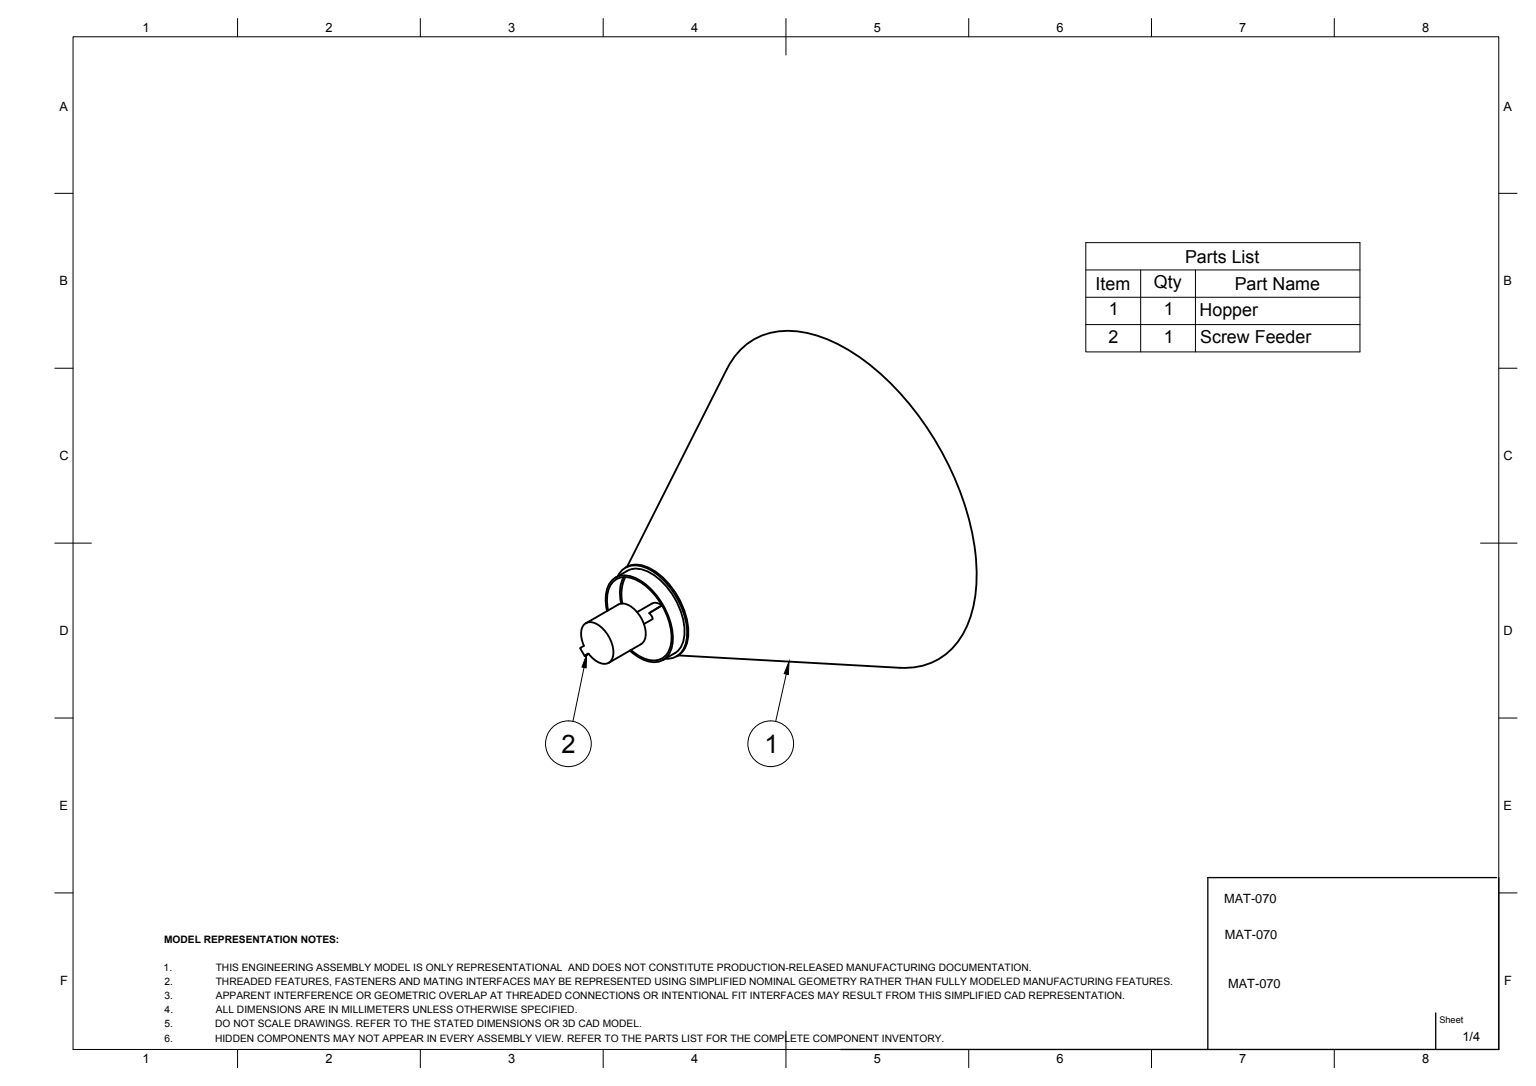
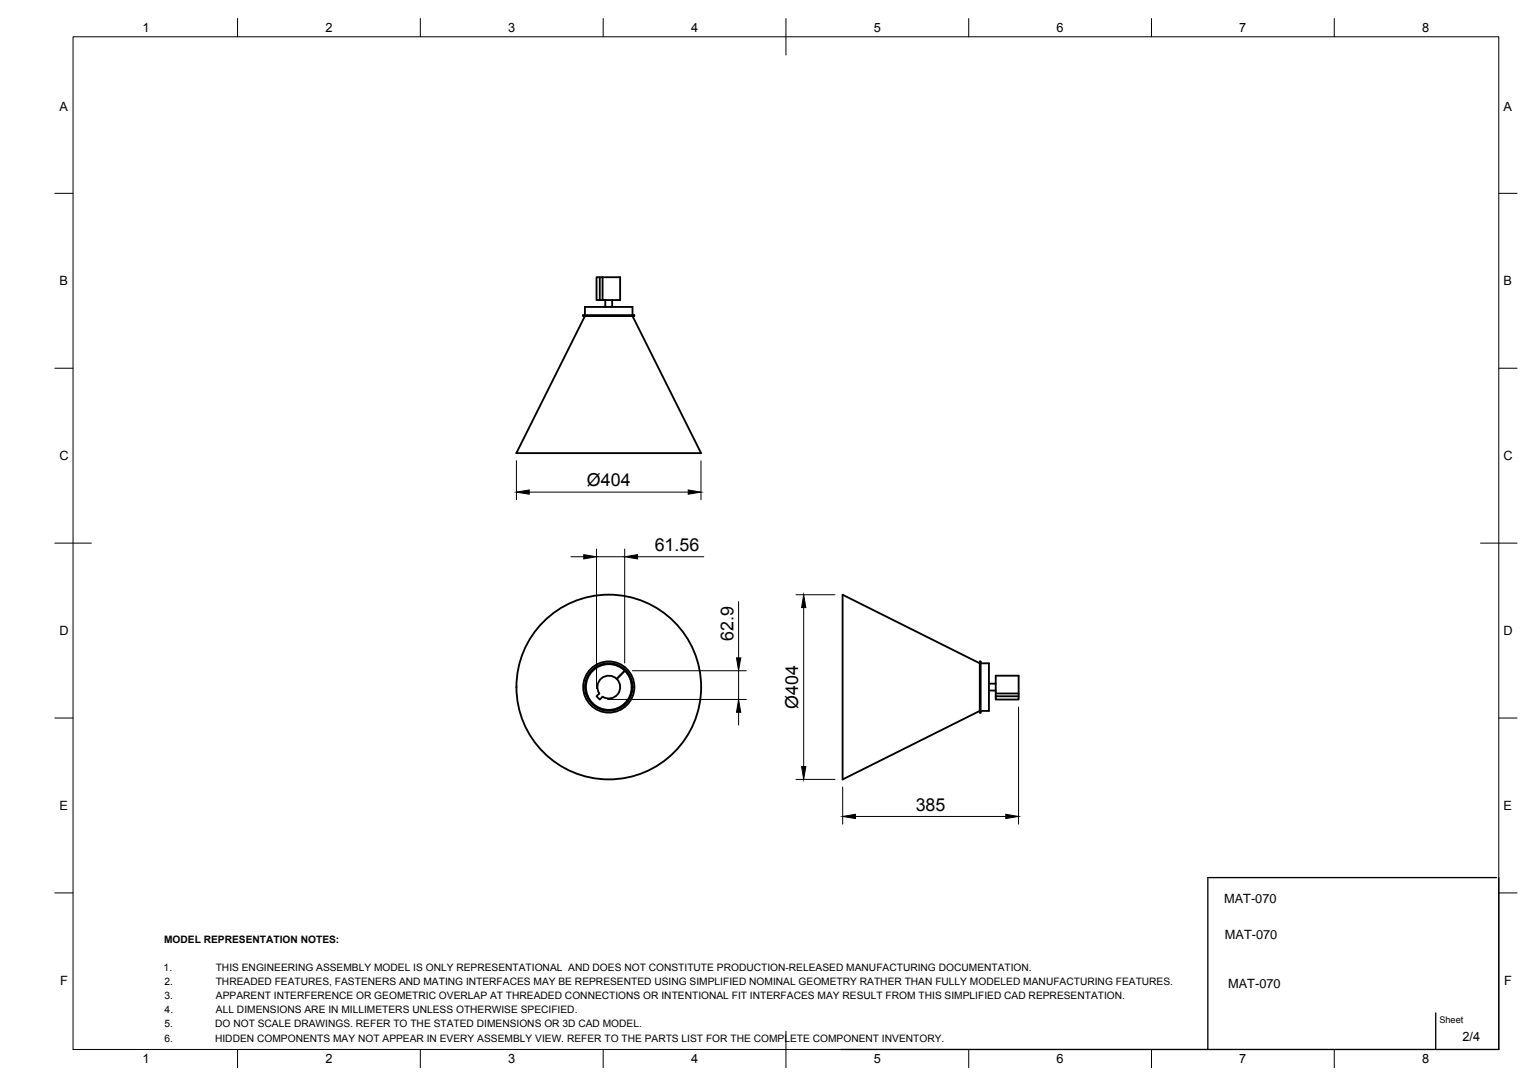
ISO-10303-21;
HEADER;
/* Generated by software containing ST-Developer
 * from STEP Tools, Inc. (www.steptools.com) 
 */

FILE_DESCRIPTION(
/* description */ (''),
/* implementation_level */ '2;1');

FILE_NAME(
/* name */ 'MAT-070',
/* time_stamp */ '2026-10-24T12:18:10-07:00',
/* author */ (''),
/* organization */ (''),
/* preprocessor_version */ 'ST-DEVELOPER v20.2',
/* originating_system */ 'Autodesk Translation Framework v15.15.0.0',
/* authorisation */ '');

FILE_SCHEMA (('AUTOMOTIVE_DESIGN { 1 0 10303 214 3 1 1 }'));
ENDSEC;

DATA;
#10=MECHANICAL_DESIGN_GEOMETRIC_PRESENTATION_REPRESENTATION('',(#38,#39),
#2858);
#11=ITEM_DEFINED_TRANSFORMATION($,$,#415,#453);
#12=ITEM_DEFINED_TRANSFORMATION($,$,#434,#454);
#13=(
REPRESENTATION_RELATIONSHIP($,$,#2872,#2871)
REPRESENTATION_RELATIONSHIP_WITH_TRANSFORMATION(#11)
SHAPE_REPRESENTATION_RELATIONSHIP()
);
#14=(
REPRESENTATION_RELATIONSHIP($,$,#2873,#2871)
REPRESENTATION_RELATIONSHIP_WITH_TRANSFORMATION(#12)
SHAPE_REPRESENTATION_RELATIONSHIP()
);
#15=CONTEXT_DEPENDENT_SHAPE_REPRESENTATION(#13,#2869);
#16=CONTEXT_DEPENDENT_SHAPE_REPRESENTATION(#14,#2870);
#17=NEXT_ASSEMBLY_USAGE_OCCURRENCE('Hopper:1','Hopper:1','Hopper:1',#2875,
#2876,'Hopper:1');
#18=NEXT_ASSEMBLY_USAGE_OCCURRENCE('Screw Feeder:1','Screw Feeder:1',
'Screw Feeder:1',#2875,#2877,'Screw Feeder:1');
#19=(
BOUNDED_SURFACE()
B_SPLINE_SURFACE(1,2,((#1855,#1856,#1857,#1858,#1859,#1860,#1861,#1862,
#1863,#1864,#1865,#1866,#1867,#1868,#1869,#1870,#1871,#1872,#1873,#1874,
#1875,#1876,#1877,#1878,#1879,#1880,#1881,#1882,#1883,#1884,#1885,#1886,
#1887,#1888,#1889,#1890,#1891,#1892,#1893,#1894,#1895,#1896,#1897,#1898,
#1899,#1900,#1901,#1902,#1903,#1904,#1905,#1906,#1907,#1908,#1909,#1910,
#1911,#1912,#1913,#1914,#1915,#1916,#1917,#1918,#1919,#1920,#1921,#1922,
#1923,#1924,#1925,#1926,#1927,#1928,#1929,#1930,#1931,#1932,#1933,#1934,
#1935,#1936,#1937,#1938,#1939,#1940,#1941,#1942,#1943,#1944,#1945,#1946,
#1947,#1948,#1949,#1950,#1951,#1952,#1953,#1954,#1955,#1956,#1957,#1958,
#1959,#1960,#1961,#1962,#1963,#1964,#1965,#1966,#1967,#1968,#1969,#1970,
#1971,#1972,#1973,#1974,#1975),(#1976,#1977,#1978,#1979,#1980,#1981,#1982,
#1983,#1984,#1985,#1986,#1987,#1988,#1989,#1990,#1991,#1992,#1993,#1994,
#1995,#1996,#1997,#1998,#1999,#2000,#2001,#2002,#2003,#2004,#2005,#2006,
#2007,#2008,#2009,#2010,#2011,#2012,#2013,#2014,#2015,#2016,#2017,#2018,
#2019,#2020,#2021,#2022,#2023,#2024,#2025,#2026,#2027,#2028,#2029,#2030,
#2031,#2032,#2033,#2034,#2035,#2036,#2037,#2038,#2039,#2040,#2041,#2042,
#2043,#2044,#2045,#2046,#2047,#2048,#2049,#2050,#2051,#2052,#2053,#2054,
#2055,#2056,#2057,#2058,#2059,#2060,#2061,#2062,#2063,#2064,#2065,#2066,
#2067,#2068,#2069,#2070,#2071,#2072,#2073,#2074,#2075,#2076,#2077,#2078,
#2079,#2080,#2081,#2082,#2083,#2084,#2085,#2086,#2087,#2088,#2089,#2090,
#2091,#2092,#2093,#2094,#2095,#2096)),.UNSPECIFIED.,.F.,.F.,.F.)
B_SPLINE_SURFACE_WITH_KNOTS((2,2),(3,2,2,2,2,2,2,2,2,2,2,2,2,2,2,2,2,2,
2,2,2,2,2,2,2,2,2,2,2,2,2,2,2,2,2,2,2,2,2,2,2,2,2,2,2,2,2,2,2,2,2,2,2,2,
2,2,2,2,2,2,3),(0.,1.),(0.,0.0166666666666667,0.0333333333333333,0.05,0.0666666666666667,
0.0833333333333333,0.1,0.116666666666667,0.133333333333333,0.15,0.166666666666667,
0.183333333333333,0.2,0.216666666666667,0.233333333333333,0.25,0.266666666666667,
0.283333333333333,0.3,0.316666666666667,0.333333333333333,0.35,0.366666666666667,
0.383333333333333,0.4,0.416666666666667,0.433333333333333,0.45,0.466666666666667,
0.483333333333333,0.5,0.516666666666667,0.533333333333333,0.55,0.566666666666667,
0.583333333333333,0.6,0.616666666666667,0.633333333333333,0.65,0.666666666666667,
0.683333333333333,0.7,0.716666666666667,0.733333333333333,0.75,0.766666666666667,
0.783333333333333,0.8,0.816666666666667,0.833333333333333,0.85,0.866666666666667,
0.883333333333333,0.9,0.916666666666667,0.933333333333333,0.95,0.966666666666667,
0.983333333333333,1.),.UNSPECIFIED.)
GEOMETRIC_REPRESENTATION_ITEM()
RATIONAL_B_SPLINE_SURFACE(((1.,0.987688340595138,1.,0.987688340595138,1.,
0.987688340595138,1.,0.987688340595138,1.,0.987688340595138,1.,0.987688340595138,
1.,0.987688340595138,1.,0.987688340595138,1.,0.987688340595138,1.,0.987688340595138,
1.,0.987688340595138,1.,0.987688340595138,1.,0.987688340595138,1.,0.987688340595138,
1.,0.987688340595138,1.,0.987688340595138,1.,0.987688340595138,1.,0.987688340595138,
1.,0.987688340595138,1.,0.987688340595138,1.,0.987688340595138,1.,0.987688340595138,
1.,0.987688340595138,1.,0.987688340595138,1.,0.987688340595138,1.,0.987688340595138,
1.,0.987688340595138,1.,0.987688340595138,1.,0.987688340595138,1.,0.987688340595138,
1.,0.987688340595138,1.,0.987688340595138,1.,0.987688340595138,1.,0.987688340595138,
1.,0.987688340595138,1.,0.987688340595138,1.,0.987688340595138,1.,0.987688340595138,
1.,0.987688340595138,1.,0.987688340595138,1.,0.987688340595138,1.,0.987688340595138,
1.,0.987688340595138,1.,0.987688340595138,1.,0.987688340595138,1.,0.987688340595138,
1.,0.987688340595138,1.,0.987688340595138,1.,0.987688340595138,1.,0.987688340595138,
1.,0.987688340595138,1.,0.987688340595138,1.,0.987688340595138,1.,0.987688340595138,
1.,0.987688340595138,1.,0.987688340595138,1.,0.987688340595138,1.,0.987688340595138,
1.,0.987688340595138,1.,0.987688340595138,1.),(1.,0.987688340595138,1.,
0.987688340595138,1.,0.987688340595138,1.,0.987688340595138,1.,0.987688340595138,
1.,0.987688340595138,1.,0.987688340595138,1.,0.987688340595138,1.,0.987688340595138,
1.,0.987688340595138,1.,0.987688340595138,1.,0.987688340595138,1.,0.987688340595138,
1.,0.987688340595138,1.,0.987688340595138,1.,0.987688340595138,1.,0.987688340595138,
1.,0.987688340595138,1.,0.987688340595138,1.,0.987688340595138,1.,0.987688340595138,
1.,0.987688340595138,1.,0.987688340595138,1.,0.987688340595138,1.,0.987688340595138,
1.,0.987688340595138,1.,0.987688340595138,1.,0.987688340595138,1.,0.987688340595138,
1.,0.987688340595138,1.,0.987688340595138,1.,0.987688340595138,1.,0.987688340595138,
1.,0.987688340595138,1.,0.987688340595138,1.,0.987688340595138,1.,0.987688340595138,
1.,0.987688340595138,1.,0.987688340595138,1.,0.987688340595138,1.,0.987688340595138,
1.,0.987688340595138,1.,0.987688340595138,1.,0.987688340595138,1.,0.987688340595138,
1.,0.987688340595138,1.,0.987688340595138,1.,0.987688340595138,1.,0.987688340595138,
1.,0.987688340595138,1.,0.987688340595138,1.,0.987688340595138,1.,0.987688340595138,
1.,0.987688340595138,1.,0.987688340595138,1.,0.987688340595138,1.,0.987688340595138,
1.,0.987688340595138,1.,0.987688340595138,1.,0.987688340595138,1.)))
REPRESENTATION_ITEM('')
SURFACE()
);
#20=(
BOUNDED_SURFACE()
B_SPLINE_SURFACE(1,2,((#2218,#2219,#2220,#2221,#2222,#2223,#2224,#2225,
#2226,#2227,#2228,#2229,#2230,#2231,#2232,#2233,#2234,#2235,#2236,#2237,
#2238,#2239,#2240,#2241,#2242,#2243,#2244,#2245,#2246,#2247,#2248,#2249,
#2250,#2251,#2252,#2253,#2254,#2255,#2256,#2257,#2258,#2259,#2260,#2261,
#2262,#2263,#2264,#2265,#2266,#2267,#2268,#2269,#2270,#2271,#2272,#2273,
#2274,#2275,#2276,#2277,#2278,#2279,#2280,#2281,#2282,#2283,#2284,#2285,
#2286,#2287,#2288,#2289,#2290,#2291,#2292,#2293,#2294,#2295,#2296,#2297,
#2298,#2299,#2300,#2301,#2302,#2303,#2304,#2305,#2306,#2307,#2308,#2309,
#2310,#2311,#2312,#2313,#2314,#2315,#2316,#2317,#2318,#2319,#2320,#2321,
#2322,#2323,#2324,#2325,#2326,#2327,#2328,#2329,#2330,#2331,#2332,#2333,
#2334,#2335,#2336,#2337,#2338),(#2339,#2340,#2341,#2342,#2343,#2344,#2345,
#2346,#2347,#2348,#2349,#2350,#2351,#2352,#2353,#2354,#2355,#2356,#2357,
#2358,#2359,#2360,#2361,#2362,#2363,#2364,#2365,#2366,#2367,#2368,#2369,
#2370,#2371,#2372,#2373,#2374,#2375,#2376,#2377,#2378,#2379,#2380,#2381,
#2382,#2383,#2384,#2385,#2386,#2387,#2388,#2389,#2390,#2391,#2392,#2393,
#2394,#2395,#2396,#2397,#2398,#2399,#2400,#2401,#2402,#2403,#2404,#2405,
#2406,#2407,#2408,#2409,#2410,#2411,#2412,#2413,#2414,#2415,#2416,#2417,
#2418,#2419,#2420,#2421,#2422,#2423,#2424,#2425,#2426,#2427,#2428,#2429,
#2430,#2431,#2432,#2433,#2434,#2435,#2436,#2437,#2438,#2439,#2440,#2441,
#2442,#2443,#2444,#2445,#2446,#2447,#2448,#2449,#2450,#2451,#2452,#2453,
#2454,#2455,#2456,#2457,#2458,#2459)),.UNSPECIFIED.,.F.,.F.,.F.)
B_SPLINE_SURFACE_WITH_KNOTS((2,2),(3,2,2,2,2,2,2,2,2,2,2,2,2,2,2,2,2,2,
2,2,2,2,2,2,2,2,2,2,2,2,2,2,2,2,2,2,2,2,2,2,2,2,2,2,2,2,2,2,2,2,2,2,2,2,
2,2,2,2,2,2,3),(0.,1.),(0.,0.0166666666666667,0.0333333333333333,0.05,0.0666666666666667,
0.0833333333333333,0.1,0.116666666666667,0.133333333333333,0.15,0.166666666666667,
0.183333333333333,0.2,0.216666666666667,0.233333333333333,0.25,0.266666666666667,
0.283333333333333,0.3,0.316666666666667,0.333333333333333,0.35,0.366666666666667,
0.383333333333333,0.4,0.416666666666667,0.433333333333333,0.45,0.466666666666667,
0.483333333333333,0.5,0.516666666666667,0.533333333333333,0.55,0.566666666666667,
0.583333333333333,0.6,0.616666666666667,0.633333333333333,0.65,0.666666666666667,
0.683333333333333,0.7,0.716666666666667,0.733333333333333,0.75,0.766666666666667,
0.783333333333333,0.8,0.816666666666667,0.833333333333333,0.85,0.866666666666667,
0.883333333333333,0.9,0.916666666666667,0.933333333333333,0.95,0.966666666666667,
0.983333333333333,1.),.UNSPECIFIED.)
GEOMETRIC_REPRESENTATION_ITEM()
RATIONAL_B_SPLINE_SURFACE(((1.,0.987688340595138,1.,0.987688340595138,1.,
0.987688340595138,1.,0.987688340595138,1.,0.987688340595138,1.,0.987688340595138,
1.,0.987688340595138,1.,0.987688340595138,1.,0.987688340595138,1.,0.987688340595138,
1.,0.987688340595138,1.,0.987688340595138,1.,0.987688340595138,1.,0.987688340595138,
1.,0.987688340595138,1.,0.987688340595138,1.,0.987688340595138,1.,0.987688340595138,
1.,0.987688340595138,1.,0.987688340595138,1.,0.987688340595138,1.,0.987688340595138,
1.,0.987688340595138,1.,0.987688340595138,1.,0.987688340595138,1.,0.987688340595138,
1.,0.987688340595138,1.,0.987688340595138,1.,0.987688340595138,1.,0.987688340595138,
1.,0.987688340595138,1.,0.987688340595138,1.,0.987688340595138,1.,0.987688340595138,
1.,0.987688340595138,1.,0.987688340595138,1.,0.987688340595138,1.,0.987688340595138,
1.,0.987688340595138,1.,0.987688340595138,1.,0.987688340595138,1.,0.987688340595138,
1.,0.987688340595138,1.,0.987688340595138,1.,0.987688340595138,1.,0.987688340595138,
1.,0.987688340595138,1.,0.987688340595138,1.,0.987688340595138,1.,0.987688340595138,
1.,0.987688340595138,1.,0.987688340595138,1.,0.987688340595138,1.,0.987688340595138,
1.,0.987688340595138,1.,0.987688340595138,1.,0.987688340595138,1.,0.987688340595138,
1.,0.987688340595138,1.,0.987688340595138,1.),(1.,0.987688340595138,1.,
0.987688340595138,1.,0.987688340595138,1.,0.987688340595138,1.,0.987688340595138,
1.,0.987688340595138,1.,0.987688340595138,1.,0.987688340595138,1.,0.987688340595138,
1.,0.987688340595138,1.,0.987688340595138,1.,0.987688340595138,1.,0.987688340595138,
1.,0.987688340595138,1.,0.987688340595138,1.,0.987688340595138,1.,0.987688340595138,
1.,0.987688340595138,1.,0.987688340595138,1.,0.987688340595138,1.,0.987688340595138,
1.,0.987688340595138,1.,0.987688340595138,1.,0.987688340595138,1.,0.987688340595138,
1.,0.987688340595138,1.,0.987688340595138,1.,0.987688340595138,1.,0.987688340595138,
1.,0.987688340595138,1.,0.987688340595138,1.,0.987688340595138,1.,0.987688340595138,
1.,0.987688340595138,1.,0.987688340595138,1.,0.987688340595138,1.,0.987688340595138,
1.,0.987688340595138,1.,0.987688340595138,1.,0.987688340595138,1.,0.987688340595138,
1.,0.987688340595138,1.,0.987688340595138,1.,0.987688340595138,1.,0.987688340595138,
1.,0.987688340595138,1.,0.987688340595138,1.,0.987688340595138,1.,0.987688340595138,
1.,0.987688340595138,1.,0.987688340595138,1.,0.987688340595138,1.,0.987688340595138,
1.,0.987688340595138,1.,0.987688340595138,1.,0.987688340595138,1.,0.987688340595138,
1.,0.987688340595138,1.,0.987688340595138,1.,0.987688340595138,1.)))
REPRESENTATION_ITEM('')
SURFACE()
);
#21=(
BOUNDED_SURFACE()
B_SPLINE_SURFACE(1,2,((#2581,#2582,#2583,#2584,#2585,#2586,#2587,#2588,
#2589,#2590,#2591,#2592,#2593,#2594,#2595,#2596,#2597,#2598,#2599,#2600,
#2601,#2602,#2603,#2604,#2605,#2606,#2607,#2608,#2609,#2610,#2611,#2612,
#2613,#2614,#2615,#2616,#2617,#2618,#2619,#2620,#2621,#2622,#2623,#2624,
#2625,#2626,#2627,#2628,#2629,#2630,#2631,#2632,#2633,#2634,#2635,#2636,
#2637,#2638,#2639,#2640,#2641,#2642,#2643,#2644,#2645,#2646,#2647,#2648,
#2649,#2650,#2651,#2652,#2653,#2654,#2655,#2656,#2657,#2658,#2659,#2660,
#2661,#2662,#2663,#2664,#2665,#2666,#2667,#2668,#2669,#2670,#2671,#2672,
#2673,#2674,#2675,#2676,#2677,#2678,#2679,#2680,#2681,#2682,#2683,#2684,
#2685,#2686,#2687,#2688,#2689,#2690,#2691,#2692,#2693,#2694,#2695,#2696,
#2697,#2698,#2699,#2700,#2701),(#2702,#2703,#2704,#2705,#2706,#2707,#2708,
#2709,#2710,#2711,#2712,#2713,#2714,#2715,#2716,#2717,#2718,#2719,#2720,
#2721,#2722,#2723,#2724,#2725,#2726,#2727,#2728,#2729,#2730,#2731,#2732,
#2733,#2734,#2735,#2736,#2737,#2738,#2739,#2740,#2741,#2742,#2743,#2744,
#2745,#2746,#2747,#2748,#2749,#2750,#2751,#2752,#2753,#2754,#2755,#2756,
#2757,#2758,#2759,#2760,#2761,#2762,#2763,#2764,#2765,#2766,#2767,#2768,
#2769,#2770,#2771,#2772,#2773,#2774,#2775,#2776,#2777,#2778,#2779,#2780,
#2781,#2782,#2783,#2784,#2785,#2786,#2787,#2788,#2789,#2790,#2791,#2792,
#2793,#2794,#2795,#2796,#2797,#2798,#2799,#2800,#2801,#2802,#2803,#2804,
#2805,#2806,#2807,#2808,#2809,#2810,#2811,#2812,#2813,#2814,#2815,#2816,
#2817,#2818,#2819,#2820,#2821,#2822)),.UNSPECIFIED.,.F.,.F.,.F.)
B_SPLINE_SURFACE_WITH_KNOTS((2,2),(3,2,2,2,2,2,2,2,2,2,2,2,2,2,2,2,2,2,
2,2,2,2,2,2,2,2,2,2,2,2,2,2,2,2,2,2,2,2,2,2,2,2,2,2,2,2,2,2,2,2,2,2,2,2,
2,2,2,2,2,2,3),(0.,1.),(0.,0.0166666666666667,0.0333333333333333,0.05,0.0666666666666667,
0.0833333333333333,0.1,0.116666666666667,0.133333333333333,0.15,0.166666666666667,
0.183333333333333,0.2,0.216666666666667,0.233333333333333,0.25,0.266666666666667,
0.283333333333333,0.3,0.316666666666667,0.333333333333333,0.35,0.366666666666667,
0.383333333333333,0.4,0.416666666666667,0.433333333333333,0.45,0.466666666666667,
0.483333333333333,0.5,0.516666666666667,0.533333333333333,0.55,0.566666666666667,
0.583333333333333,0.6,0.616666666666667,0.633333333333333,0.65,0.666666666666667,
0.683333333333333,0.7,0.716666666666667,0.733333333333333,0.75,0.766666666666667,
0.783333333333333,0.8,0.816666666666667,0.833333333333333,0.85,0.866666666666667,
0.883333333333333,0.9,0.916666666666667,0.933333333333333,0.95,0.966666666666667,
0.983333333333333,1.),.UNSPECIFIED.)
GEOMETRIC_REPRESENTATION_ITEM()
RATIONAL_B_SPLINE_SURFACE(((1.,0.987688340595138,1.,0.987688340595138,1.,
0.987688340595138,1.,0.987688340595138,1.,0.987688340595138,1.,0.987688340595138,
1.,0.987688340595138,1.,0.987688340595138,1.,0.987688340595138,1.,0.987688340595138,
1.,0.987688340595138,1.,0.987688340595138,1.,0.987688340595138,1.,0.987688340595138,
1.,0.987688340595138,1.,0.987688340595138,1.,0.987688340595138,1.,0.987688340595138,
1.,0.987688340595138,1.,0.987688340595138,1.,0.987688340595138,1.,0.987688340595138,
1.,0.987688340595138,1.,0.987688340595138,1.,0.987688340595138,1.,0.987688340595138,
1.,0.987688340595138,1.,0.987688340595138,1.,0.987688340595138,1.,0.987688340595138,
1.,0.987688340595138,1.,0.987688340595138,1.,0.987688340595138,1.,0.987688340595138,
1.,0.987688340595138,1.,0.987688340595138,1.,0.987688340595138,1.,0.987688340595138,
1.,0.987688340595138,1.,0.987688340595138,1.,0.987688340595138,1.,0.987688340595138,
1.,0.987688340595138,1.,0.987688340595138,1.,0.987688340595138,1.,0.987688340595138,
1.,0.987688340595138,1.,0.987688340595138,1.,0.987688340595138,1.,0.987688340595138,
1.,0.987688340595138,1.,0.987688340595138,1.,0.987688340595138,1.,0.987688340595138,
1.,0.987688340595138,1.,0.987688340595138,1.,0.987688340595138,1.,0.987688340595138,
1.,0.987688340595138,1.,0.987688340595138,1.),(1.,0.987688340595138,1.,
0.987688340595138,1.,0.987688340595138,1.,0.987688340595138,1.,0.987688340595138,
1.,0.987688340595138,1.,0.987688340595138,1.,0.987688340595138,1.,0.987688340595138,
1.,0.987688340595138,1.,0.987688340595138,1.,0.987688340595138,1.,0.987688340595138,
1.,0.987688340595138,1.,0.987688340595138,1.,0.987688340595138,1.,0.987688340595138,
1.,0.987688340595138,1.,0.987688340595138,1.,0.987688340595138,1.,0.987688340595138,
1.,0.987688340595138,1.,0.987688340595138,1.,0.987688340595138,1.,0.987688340595138,
1.,0.987688340595138,1.,0.987688340595138,1.,0.987688340595138,1.,0.987688340595138,
1.,0.987688340595138,1.,0.987688340595138,1.,0.987688340595138,1.,0.987688340595138,
1.,0.987688340595138,1.,0.987688340595138,1.,0.987688340595138,1.,0.987688340595138,
1.,0.987688340595138,1.,0.987688340595138,1.,0.987688340595138,1.,0.987688340595138,
1.,0.987688340595138,1.,0.987688340595138,1.,0.987688340595138,1.,0.987688340595138,
1.,0.987688340595138,1.,0.987688340595138,1.,0.987688340595138,1.,0.987688340595138,
1.,0.987688340595138,1.,0.987688340595138,1.,0.987688340595138,1.,0.987688340595138,
1.,0.987688340595138,1.,0.987688340595138,1.,0.987688340595138,1.,0.987688340595138,
1.,0.987688340595138,1.,0.987688340595138,1.,0.987688340595138,1.)))
REPRESENTATION_ITEM('')
SURFACE()
);
#22=B_SPLINE_CURVE_WITH_KNOTS('',3,(#652,#653,#654,#655),.UNSPECIFIED.,
 .F.,.F.,(4,4),(-1.,-0.998645968698766),.UNSPECIFIED.);
#23=B_SPLINE_CURVE_WITH_KNOTS('',3,(#662,#663,#664,#665,#666,#667,#668,
#669,#670,#671,#672,#673,#674,#675,#676,#677,#678,#679,#680,#681,#682,#683,
#684,#685,#686,#687,#688,#689,#690,#691,#692,#693,#694,#695,#696,#697,#698,
#699,#700,#701,#702,#703,#704,#705,#706,#707,#708,#709,#710,#711,#712,#713,
#714,#715,#716,#717,#718,#719,#720,#721,#722,#723,#724,#725,#726,#727,#728,
#729,#730,#731,#732,#733,#734,#735,#736,#737,#738,#739,#740,#741,#742,#743,
#744,#745,#746,#747,#748,#749,#750,#751,#752,#753,#754,#755,#756,#757,#758,
#759,#760,#761,#762,#763,#764,#765,#766,#767,#768,#769,#770,#771,#772,#773,
#774,#775,#776,#777,#778,#779,#780,#781,#782,#783,#784,#785,#786,#787,#788,
#789,#790,#791,#792,#793,#794,#795,#796,#797,#798,#799,#800,#801,#802,#803,
#804,#805,#806,#807,#808,#809,#810,#811,#812,#813,#814,#815,#816,#817,#818,
#819,#820,#821,#822,#823,#824,#825,#826,#827,#828,#829,#830,#831,#832,#833,
#834,#835,#836,#837,#838,#839,#840,#841,#842,#843,#844,#845,#846,#847,#848,
#849,#850,#851,#852,#853,#854,#855,#856,#857,#858,#859,#860,#861,#862,#863,
#864,#865,#866,#867,#868,#869,#870,#871,#872,#873,#874,#875,#876,#877,#878,
#879,#880,#881,#882,#883,#884,#885,#886,#887,#888,#889,#890,#891,#892,#893,
#894,#895,#896,#897,#898,#899,#900,#901,#902,#903,#904,#905,#906,#907,#908,
#909,#910,#911,#912,#913,#914,#915,#916,#917,#918,#919,#920,#921,#922,#923,
#924,#925,#926,#927,#928,#929,#930,#931,#932,#933,#934,#935,#936,#937,#938,
#939,#940,#941,#942,#943,#944,#945,#946,#947,#948,#949,#950,#951,#952,#953,
#954,#955,#956,#957,#958,#959,#960,#961,#962,#963,#964,#965,#966,#967,#968,
#969,#970,#971,#972,#973,#974,#975,#976,#977,#978,#979,#980,#981,#982,#983,
#984,#985,#986,#987,#988,#989,#990,#991,#992,#993,#994,#995,#996,#997,#998,
#999,#1000,#1001,#1002,#1003,#1004,#1005,#1006,#1007,#1008,#1009,#1010,
#1011,#1012,#1013,#1014,#1015,#1016,#1017,#1018,#1019),.UNSPECIFIED.,.F.,
 .F.,(4,3,3,3,3,3,3,3,3,3,3,3,3,3,3,3,3,3,3,3,3,3,3,3,3,3,3,3,3,3,3,3,3,
3,3,3,3,3,3,3,3,3,3,3,3,3,3,3,3,3,3,3,3,3,3,3,3,3,3,3,3,3,3,3,3,3,3,3,3,
3,3,3,3,3,3,3,3,3,3,3,3,3,3,3,3,3,3,3,3,3,3,3,3,3,3,3,3,3,3,3,3,3,3,3,3,
3,3,3,3,3,3,3,3,3,3,3,3,3,3,4),(-0.331979302032099,-0.328745544947817,-0.325511126349503,
-0.322277581756429,-0.319042795051795,-0.316666666666667,-0.313432410645245,
-0.310074307983934,-0.306840488099785,-0.303607230746873,-0.300373105768056,
-0.3,-0.296765743978578,-0.293407641317267,-0.290173821433118,-0.286940564080179,
-0.283706439101408,-0.283333333333333,-0.280099077311897,-0.27674097465059,
-0.273507154766441,-0.270273897413541,-0.267039772434759,-0.266666666666667,
-0.263432410645244,-0.260074307983933,-0.25684048809978,-0.253607230746841,
-0.250373105768036,-0.25,-0.246765743978575,-0.243407641317264,-0.240173821433105,
-0.236940564080198,-0.233706439101398,-0.233333333333333,-0.230099077311924,
-0.22674097465061,-0.223507154766454,-0.220273897413536,-0.217039772434708,
-0.216666666666667,-0.213432410645268,-0.210074307983951,-0.206840488099798,
-0.203607230746877,-0.200373105768084,-0.2,-0.196765743978578,-0.193407641317267,
-0.190173821433123,-0.186940564080229,-0.183706439101414,-0.183333333333333,
-0.180099077311908,-0.176740974650597,-0.173507154766428,-0.170273897413483,
-0.167039772434678,-0.166666666666667,-0.163432410645259,-0.160074307983944,
-0.156840488099797,-0.153607230746853,-0.150373105768069,-0.15,-0.146765743978574,
-0.143407641317264,-0.140173821433101,-0.136940564080169,-0.133706439101386,
-0.133333333333333,-0.130099077311911,-0.1267409746506,-0.123507154766447,
-0.120273897413526,-0.117039772434722,-0.116666666666667,-0.113432410645241,
-0.110074307983931,-0.106840488099774,-0.103607230746858,-0.10037310576804,
-0.1,-0.0967657439785776,-0.0934076413172665,-0.0901738214331063,-0.0869405640801917,
-0.0837064391013879,-0.0833333333333334,-0.0800990773119075,-0.0767409746505973,
-0.0735071547664396,-0.0702738974135466,-0.0670397724347522,-0.0666666666666667,
-0.0634324106452447,-0.0600743079839336,-0.0568404880997839,-0.0536072307468639,
-0.0503731057680767,-0.05,-0.0467657439785748,-0.0434076413172644,-0.0401738214331216,
-0.0369405640801967,-0.033706439101418,-0.0333333333333333,-0.030099077311911,
-0.0267409746505999,-0.0235071547664523,-0.0202738974135343,-0.017039772434738,
-0.0166666666666667,-0.0134324106517174,-0.0100743318149406,-0.00684051195133032,
-0.00360725461687006,-0.000373129688631168,-9.53046099950368E-8),
 .UNSPECIFIED.);
#24=B_SPLINE_CURVE_WITH_KNOTS('',3,(#1066,#1067,#1068,#1069,#1070,#1071,
#1072,#1073,#1074,#1075,#1076,#1077,#1078,#1079,#1080,#1081,#1082,#1083,
#1084,#1085,#1086,#1087,#1088,#1089,#1090,#1091,#1092,#1093,#1094,#1095,
#1096,#1097,#1098,#1099,#1100,#1101,#1102,#1103,#1104,#1105,#1106,#1107,
#1108,#1109,#1110,#1111,#1112,#1113,#1114,#1115,#1116,#1117,#1118,#1119,
#1120,#1121,#1122,#1123,#1124,#1125,#1126,#1127,#1128,#1129,#1130,#1131,
#1132,#1133,#1134,#1135,#1136,#1137,#1138,#1139,#1140,#1141,#1142,#1143,
#1144,#1145,#1146,#1147,#1148,#1149,#1150,#1151,#1152,#1153,#1154,#1155,
#1156,#1157,#1158,#1159,#1160,#1161,#1162,#1163,#1164,#1165,#1166,#1167,
#1168,#1169,#1170,#1171,#1172,#1173,#1174,#1175,#1176,#1177,#1178,#1179,
#1180,#1181,#1182,#1183,#1184,#1185,#1186,#1187,#1188,#1189,#1190,#1191,
#1192,#1193,#1194,#1195,#1196,#1197,#1198,#1199,#1200,#1201,#1202,#1203,
#1204,#1205,#1206,#1207,#1208,#1209,#1210,#1211,#1212,#1213,#1214,#1215,
#1216,#1217,#1218,#1219,#1220,#1221,#1222,#1223,#1224,#1225,#1226,#1227,
#1228,#1229,#1230,#1231,#1232,#1233,#1234,#1235,#1236,#1237,#1238,#1239,
#1240,#1241,#1242,#1243,#1244,#1245,#1246,#1247,#1248,#1249,#1250,#1251,
#1252,#1253,#1254,#1255,#1256,#1257,#1258,#1259,#1260,#1261,#1262,#1263,
#1264,#1265,#1266,#1267,#1268,#1269,#1270,#1271,#1272,#1273,#1274,#1275,
#1276,#1277,#1278,#1279,#1280,#1281,#1282,#1283,#1284,#1285,#1286,#1287,
#1288,#1289,#1290,#1291,#1292,#1293,#1294,#1295,#1296,#1297,#1298,#1299,
#1300,#1301,#1302,#1303,#1304,#1305,#1306,#1307,#1308,#1309,#1310,#1311,
#1312,#1313,#1314,#1315,#1316,#1317,#1318,#1319,#1320,#1321,#1322,#1323,
#1324,#1325,#1326,#1327,#1328,#1329,#1330,#1331,#1332,#1333,#1334,#1335,
#1336,#1337,#1338,#1339,#1340,#1341,#1342,#1343,#1344,#1345,#1346,#1347,
#1348,#1349,#1350,#1351,#1352,#1353,#1354,#1355,#1356,#1357,#1358,#1359,
#1360,#1361,#1362,#1363,#1364,#1365,#1366,#1367,#1368,#1369,#1370,#1371,
#1372,#1373,#1374,#1375,#1376,#1377,#1378,#1379,#1380,#1381,#1382,#1383,
#1384,#1385,#1386,#1387,#1388,#1389,#1390,#1391,#1392,#1393,#1394,#1395,
#1396,#1397,#1398,#1399,#1400,#1401,#1402,#1403,#1404,#1405,#1406,#1407,
#1408,#1409,#1410,#1411,#1412,#1413,#1414,#1415,#1416,#1417,#1418,#1419,
#1420,#1421,#1422,#1423,#1424,#1425,#1426),.UNSPECIFIED.,.F.,.F.,(4,3,3,
3,3,3,3,3,3,3,3,3,3,3,3,3,3,3,3,3,3,3,3,3,3,3,3,3,3,3,3,3,3,3,3,3,3,3,3,
3,3,3,3,3,3,3,3,3,3,3,3,3,3,3,3,3,3,3,3,3,3,3,3,3,3,3,3,3,3,3,3,3,3,3,3,
3,3,3,3,3,3,3,3,3,3,3,3,3,3,3,3,3,3,3,3,3,3,3,3,3,3,3,3,3,3,3,3,3,3,3,3,
3,3,3,3,3,3,3,3,3,4),(-0.665312635365433,-0.662078878281142,-0.658844459682826,
-0.655610915089758,-0.652376128385123,-0.65,-0.646765743978579,-0.643407641317267,
-0.640173821433118,-0.636940564080195,-0.633706439101402,-0.633333333333333,
-0.630099077311912,-0.626740974650601,-0.623507154766448,-0.620273897413523,
-0.617039772434729,-0.616666666666667,-0.613432410645243,-0.610074307983932,
-0.60684048809978,-0.603607230746855,-0.60037310576806,-0.6,-0.596765743978578,
-0.593407641317267,-0.590173821433114,-0.586940564080189,-0.583706439101395,
-0.583333333333333,-0.580099077311911,-0.5767409746506,-0.573507154766447,
-0.570273897413521,-0.567039772434727,-0.566666666666667,-0.563432410645245,
-0.560074307983934,-0.556840488099781,-0.553607230746856,-0.550373105768065,
-0.55,-0.546765743978579,-0.543407641317267,-0.540173821433115,-0.536940564080189,
-0.533706439101384,-0.533333333333333,-0.530099077311911,-0.5267409746506,
-0.523507154766446,-0.52027389741352,-0.517039772434727,-0.516666666666667,
-0.513432410645245,-0.510074307983934,-0.506840488099781,-0.503607230746855,
-0.500373105768063,-0.5,-0.496765743978578,-0.493407641317267,-0.490173821433103,
-0.486940564080178,-0.483706439101384,-0.483333333333333,-0.480099077311911,
-0.4767409746506,-0.473507154766447,-0.47027389741351,-0.467039772434717,
-0.466666666666667,-0.463432410645245,-0.460074307983933,-0.456840488099777,
-0.453607230746852,-0.450373105768059,-0.45,-0.446765743978577,-0.443407641317266,
-0.440173821433109,-0.43694056408017,-0.433706439101377,-0.433333333333333,
-0.430099077311911,-0.4267409746506,-0.423507154766447,-0.420273897413509,
-0.417039772434716,-0.416666666666667,-0.413432410645244,-0.410074307983933,
-0.40684048809978,-0.403607230746867,-0.400373105768075,-0.4,-0.396765743978578,
-0.393407641317267,-0.390173821433118,-0.386940564080206,-0.383706439101414,
-0.383333333333333,-0.380099077311912,-0.376740974650601,-0.373507154766456,
-0.370273897413568,-0.367039772434754,-0.366666666666667,-0.363432410645244,
-0.360074307983933,-0.356840488099784,-0.353607230746845,-0.350373105768042,
-0.35,-0.346765743978578,-0.343407641317267,-0.34017382143311,-0.336940564080171,
-0.333706439101378,-0.333333333333333,-0.331979302032099),.UNSPECIFIED.);
#25=B_SPLINE_CURVE_WITH_KNOTS('',3,(#1472,#1473,#1474,#1475,#1476,#1477,
#1478,#1479,#1480,#1481,#1482,#1483,#1484,#1485,#1486,#1487,#1488,#1489,
#1490,#1491,#1492,#1493,#1494,#1495,#1496,#1497,#1498,#1499,#1500,#1501,
#1502,#1503,#1504,#1505,#1506,#1507,#1508,#1509,#1510,#1511,#1512,#1513,
#1514,#1515,#1516,#1517,#1518,#1519,#1520,#1521,#1522,#1523,#1524,#1525,
#1526,#1527,#1528,#1529,#1530,#1531,#1532,#1533,#1534,#1535,#1536,#1537,
#1538,#1539,#1540,#1541,#1542,#1543,#1544,#1545,#1546,#1547,#1548,#1549,
#1550,#1551,#1552,#1553,#1554,#1555,#1556,#1557,#1558,#1559,#1560,#1561,
#1562,#1563,#1564,#1565,#1566,#1567,#1568,#1569,#1570,#1571,#1572,#1573,
#1574,#1575,#1576,#1577,#1578,#1579,#1580,#1581,#1582,#1583,#1584,#1585,
#1586,#1587,#1588,#1589,#1590,#1591,#1592,#1593,#1594,#1595,#1596,#1597,
#1598,#1599,#1600,#1601,#1602,#1603,#1604,#1605,#1606,#1607,#1608,#1609,
#1610,#1611,#1612,#1613,#1614,#1615,#1616,#1617,#1618,#1619,#1620,#1621,
#1622,#1623,#1624,#1625,#1626,#1627,#1628,#1629,#1630,#1631,#1632,#1633,
#1634,#1635,#1636,#1637,#1638,#1639,#1640,#1641,#1642,#1643,#1644,#1645,
#1646,#1647,#1648,#1649,#1650,#1651,#1652,#1653,#1654,#1655,#1656,#1657,
#1658,#1659,#1660,#1661,#1662,#1663,#1664,#1665,#1666,#1667,#1668,#1669,
#1670,#1671,#1672,#1673,#1674,#1675,#1676,#1677,#1678,#1679,#1680,#1681,
#1682,#1683,#1684,#1685,#1686,#1687,#1688,#1689,#1690,#1691,#1692,#1693,
#1694,#1695,#1696,#1697,#1698,#1699,#1700,#1701,#1702,#1703,#1704,#1705,
#1706,#1707,#1708,#1709,#1710,#1711,#1712,#1713,#1714,#1715,#1716,#1717,
#1718,#1719,#1720,#1721,#1722,#1723,#1724,#1725,#1726,#1727,#1728,#1729,
#1730,#1731,#1732,#1733,#1734,#1735,#1736,#1737,#1738,#1739,#1740,#1741,
#1742,#1743,#1744,#1745,#1746,#1747,#1748,#1749,#1750,#1751,#1752,#1753,
#1754,#1755,#1756,#1757,#1758,#1759,#1760,#1761,#1762,#1763,#1764,#1765,
#1766,#1767,#1768,#1769,#1770,#1771,#1772,#1773,#1774,#1775,#1776,#1777,
#1778,#1779,#1780,#1781,#1782,#1783,#1784,#1785,#1786,#1787,#1788,#1789,
#1790,#1791,#1792,#1793,#1794,#1795,#1796,#1797,#1798,#1799,#1800,#1801,
#1802,#1803,#1804,#1805,#1806,#1807,#1808,#1809,#1810,#1811,#1812,#1813,
#1814,#1815,#1816,#1817,#1818,#1819,#1820,#1821,#1822,#1823,#1824,#1825,
#1826,#1827,#1828,#1829,#1830,#1831,#1832),.UNSPECIFIED.,.F.,.F.,(4,3,3,
3,3,3,3,3,3,3,3,3,3,3,3,3,3,3,3,3,3,3,3,3,3,3,3,3,3,3,3,3,3,3,3,3,3,3,3,
3,3,3,3,3,3,3,3,3,3,3,3,3,3,3,3,3,3,3,3,3,3,3,3,3,3,3,3,3,3,3,3,3,3,3,3,
3,3,3,3,3,3,3,3,3,3,3,3,3,3,3,3,3,3,3,3,3,3,3,3,3,3,3,3,3,3,3,3,3,3,3,3,
3,3,3,3,3,3,3,3,3,4),(-0.998645968698766,-0.995412211614476,-0.99217779301616,
-0.988944248423087,-0.985709461718452,-0.983333333333333,-0.980099077311911,
-0.9767409746506,-0.973507154766447,-0.970273897413519,-0.967039772434726,
-0.966666666666667,-0.963432410645243,-0.960074307983932,-0.956840488099779,
-0.953607230746854,-0.950373105768062,-0.95,-0.946765743978577,-0.943407641317266,
-0.940173821433113,-0.936940564080185,-0.933706439101392,-0.933333333333333,
-0.930099077311911,-0.9267409746506,-0.923507154766446,-0.92027389741352,
-0.917039772434728,-0.916666666666667,-0.913432410645244,-0.910074307983933,
-0.90684048809978,-0.903607230746854,-0.90037310576806,-0.9,-0.896765743978578,
-0.893407641317267,-0.890173821433115,-0.886940564080189,-0.883706439101396,
-0.883333333333333,-0.880099077311911,-0.8767409746506,-0.873507154766449,
-0.870273897413525,-0.867039772434733,-0.866666666666667,-0.863432410645245,
-0.860074307983934,-0.856840488099781,-0.853607230746854,-0.850373105768058,
-0.85,-0.846765743978578,-0.843407641317267,-0.840173821433114,-0.836940564080188,
-0.833706439101395,-0.833333333333333,-0.830099077311911,-0.8267409746506,
-0.823507154766447,-0.820273897413526,-0.817039772434731,-0.816666666666667,
-0.81343241064524,-0.81007430798393,-0.806840488099777,-0.803607230746853,
-0.800373105768059,-0.8,-0.796765743978579,-0.793407641317267,-0.790173821433115,
-0.786940564080183,-0.783706439101388,-0.783333333333333,-0.780099077311911,
-0.7767409746506,-0.773507154766446,-0.770273897413509,-0.767039772434712,
-0.766666666666667,-0.763432410645249,-0.760074307983936,-0.756840488099782,
-0.753607230746868,-0.75037310576807,-0.75,-0.746765743978578,-0.743407641317267,
-0.740173821433118,-0.736940564080168,-0.733706439101356,-0.733333333333333,
-0.730099077311911,-0.7267409746506,-0.723507154766451,-0.720273897413524,
-0.717039772434739,-0.716666666666667,-0.713432410645237,-0.710074307983928,
-0.706840488099775,-0.703607230746849,-0.700373105768067,-0.7,-0.69676574397857,
-0.693407641317261,-0.690173821433107,-0.686940564080183,-0.683706439101389,
-0.683333333333333,-0.680099077311912,-0.6767409746506,-0.673507154766448,
-0.670273897413522,-0.667039772434727,-0.666666666666667,-0.665312635365433),
 .UNSPECIFIED.);
#26=B_SPLINE_CURVE_WITH_KNOTS('',3,(#1835,#1836,#1837,#1838,#1839,#1840),
 .UNSPECIFIED.,.F.,.F.,(4,2,4),(-4.25163970020424,-2.12588055073164,0.),
 .UNSPECIFIED.);
#27=B_SPLINE_CURVE_WITH_KNOTS('',3,(#1846,#1847,#1848,#1849,#1850,#1851),
 .UNSPECIFIED.,.F.,.F.,(4,2,4),(-4.25163970020424,-2.1257591494726,0.),
 .UNSPECIFIED.);
#28=(
BOUNDED_CURVE()
B_SPLINE_CURVE(2,(#600,#601,#602,#603,#604,#605,#606,#607,#608,#609,#610,
#611,#612,#613,#614,#615,#616,#617,#618,#619,#620,#621,#622,#623,#624,#625,
#626,#627,#628,#629,#630,#631,#632,#633,#634,#635,#636,#637,#638,#639,#640,
#641,#642),.UNSPECIFIED.,.F.,.F.)
B_SPLINE_CURVE_WITH_KNOTS((3,2,2,2,2,2,2,2,2,2,2,2,2,2,2,2,2,2,2,2,2,3),
(1.82334519084262E-6,0.0166666666666667,0.0333333333333333,0.05,0.0666666666666667,
0.0833333333333333,0.1,0.116666666666667,0.133333333333333,0.15,0.166666666666667,
0.183333333333333,0.2,0.216666666666667,0.233333333333333,0.25,0.266666666666667,
0.283333333333333,0.3,0.316666666666667,0.333333333333333,0.333335156678524),
 .UNSPECIFIED.)
CURVE()
GEOMETRIC_REPRESENTATION_ITEM()
RATIONAL_B_SPLINE_CURVE((0.999997306486108,0.987689687499436,1.,0.987688340595138,
1.,0.987688340595138,1.,0.987688340595138,1.,0.987688340595138,1.,0.987688340595138,
1.,0.987688340595138,1.,0.987688340595138,1.,0.987688340595138,1.,0.987688340595138,
1.,0.987688340595138,1.,0.987688340595138,1.,0.987688340595138,1.,0.987688340595138,
1.,0.987688340595138,1.,0.987688340595138,1.,0.987688340595138,1.,0.987688340595138,
1.,0.987688340595138,1.,0.987688340595138,1.,0.999998653095702,0.999997306486109))
REPRESENTATION_ITEM('')
);
#29=(
BOUNDED_CURVE()
B_SPLINE_CURVE(2,(#647,#648,#649),.UNSPECIFIED.,.F.,.F.)
B_SPLINE_CURVE_WITH_KNOTS((3,3),(0.,1.82334519084262E-6),.UNSPECIFIED.)
CURVE()
GEOMETRIC_REPRESENTATION_ITEM()
RATIONAL_B_SPLINE_CURVE((1.,0.999998653095702,0.999997306486108))
REPRESENTATION_ITEM('')
);
#30=(
BOUNDED_CURVE()
B_SPLINE_CURVE(2,(#1023,#1024,#1025,#1026,#1027,#1028,#1029,#1030,#1031,
#1032,#1033,#1034,#1035,#1036,#1037,#1038,#1039,#1040,#1041,#1042,#1043,
#1044,#1045,#1046,#1047,#1048,#1049,#1050,#1051,#1052,#1053,#1054,#1055,
#1056,#1057,#1058,#1059,#1060,#1061,#1062,#1063),.UNSPECIFIED.,.F.,.F.)
B_SPLINE_CURVE_WITH_KNOTS((3,2,2,2,2,2,2,2,2,2,2,2,2,2,2,2,2,2,2,2,3),(0.666668490011857,
0.683333333333333,0.7,0.716666666666667,0.733333333333333,0.75,0.766666666666667,
0.783333333333333,0.8,0.816666666666667,0.833333333333333,0.85,0.866666666666667,
0.883333333333333,0.9,0.916666666666667,0.933333333333333,0.95,0.966666666666667,
0.983333333333333,1.),.UNSPECIFIED.)
CURVE()
GEOMETRIC_REPRESENTATION_ITEM()
RATIONAL_B_SPLINE_CURVE((0.999997306486109,0.987689687499436,1.,0.987688340595138,
1.,0.987688340595138,1.,0.987688340595138,1.,0.987688340595138,1.,0.987688340595138,
1.,0.987688340595138,1.,0.987688340595138,1.,0.987688340595138,1.,0.987688340595138,
1.,0.987688340595138,1.,0.987688340595138,1.,0.987688340595138,1.,0.987688340595138,
1.,0.987688340595138,1.,0.987688340595138,1.,0.987688340595138,1.,0.987688340595138,
1.,0.987688340595138,1.,0.987688340595138,1.))
REPRESENTATION_ITEM('')
);
#31=(
BOUNDED_CURVE()
B_SPLINE_CURVE(2,(#1429,#1430,#1431,#1432,#1433,#1434,#1435,#1436,#1437,
#1438,#1439,#1440,#1441,#1442,#1443,#1444,#1445,#1446,#1447,#1448,#1449,
#1450,#1451,#1452,#1453,#1454,#1455,#1456,#1457,#1458,#1459,#1460,#1461,
#1462,#1463,#1464,#1465,#1466,#1467,#1468,#1469,#1470,#1471),
 .UNSPECIFIED.,.F.,.F.)
B_SPLINE_CURVE_WITH_KNOTS((3,2,2,2,2,2,2,2,2,2,2,2,2,2,2,2,2,2,2,2,2,3),
(0.333335156678524,0.35,0.366666666666667,0.383333333333333,0.4,0.416666666666667,
0.433333333333333,0.45,0.466666666666667,0.483333333333333,0.5,0.516666666666667,
0.533333333333333,0.55,0.566666666666667,0.583333333333333,0.6,0.616666666666667,
0.633333333333333,0.65,0.666666666666667,0.666668490011857),
 .UNSPECIFIED.)
CURVE()
GEOMETRIC_REPRESENTATION_ITEM()
RATIONAL_B_SPLINE_CURVE((0.999997306486109,0.987689687499436,1.,0.987688340595138,
1.,0.987688340595138,1.,0.987688340595138,1.,0.987688340595138,1.,0.987688340595138,
1.,0.987688340595138,1.,0.987688340595138,1.,0.987688340595138,1.,0.987688340595138,
1.,0.987688340595138,1.,0.987688340595138,1.,0.987688340595138,1.,0.987688340595138,
1.,0.987688340595138,1.,0.987688340595138,1.,0.987688340595138,1.,0.987688340595138,
1.,0.987688340595138,1.,0.987688340595138,1.,0.999998653095702,0.999997306486109))
REPRESENTATION_ITEM('')
);
#32=(
BOUNDED_CURVE()
B_SPLINE_CURVE(2,(#2097,#2098,#2099,#2100,#2101,#2102,#2103,#2104,#2105,
#2106,#2107,#2108,#2109,#2110,#2111,#2112,#2113,#2114,#2115,#2116,#2117,
#2118,#2119,#2120,#2121,#2122,#2123,#2124,#2125,#2126,#2127,#2128,#2129,
#2130,#2131,#2132,#2133,#2134,#2135,#2136,#2137,#2138,#2139,#2140,#2141,
#2142,#2143,#2144,#2145,#2146,#2147,#2148,#2149,#2150,#2151,#2152,#2153,
#2154,#2155,#2156,#2157,#2158,#2159,#2160,#2161,#2162,#2163,#2164,#2165,
#2166,#2167,#2168,#2169,#2170,#2171,#2172,#2173,#2174,#2175,#2176,#2177,
#2178,#2179,#2180,#2181,#2182,#2183,#2184,#2185,#2186,#2187,#2188,#2189,
#2190,#2191,#2192,#2193,#2194,#2195,#2196,#2197,#2198,#2199,#2200,#2201,
#2202,#2203,#2204,#2205,#2206,#2207,#2208,#2209,#2210,#2211,#2212,#2213,
#2214,#2215,#2216,#2217),.UNSPECIFIED.,.F.,.F.)
B_SPLINE_CURVE_WITH_KNOTS((3,2,2,2,2,2,2,2,2,2,2,2,2,2,2,2,2,2,2,2,2,2,
2,2,2,2,2,2,2,2,2,2,2,2,2,2,2,2,2,2,2,2,2,2,2,2,2,2,2,2,2,2,2,2,2,2,2,2,
2,2,3),(0.,0.0166666666666667,0.0333333333333333,0.05,0.0666666666666667,
0.0833333333333333,0.1,0.116666666666667,0.133333333333333,0.15,0.166666666666667,
0.183333333333333,0.2,0.216666666666667,0.233333333333333,0.25,0.266666666666667,
0.283333333333333,0.3,0.316666666666667,0.333333333333333,0.35,0.366666666666667,
0.383333333333333,0.4,0.416666666666667,0.433333333333333,0.45,0.466666666666667,
0.483333333333333,0.5,0.516666666666667,0.533333333333333,0.55,0.566666666666667,
0.583333333333333,0.6,0.616666666666667,0.633333333333333,0.65,0.666666666666667,
0.683333333333333,0.7,0.716666666666667,0.733333333333333,0.75,0.766666666666667,
0.783333333333333,0.8,0.816666666666667,0.833333333333333,0.85,0.866666666666667,
0.883333333333333,0.9,0.916666666666667,0.933333333333333,0.95,0.966666666666667,
0.983333333333333,1.),.UNSPECIFIED.)
CURVE()
GEOMETRIC_REPRESENTATION_ITEM()
RATIONAL_B_SPLINE_CURVE((1.,0.987688340595138,1.,0.987688340595138,1.,0.987688340595138,
1.,0.987688340595138,1.,0.987688340595138,1.,0.987688340595138,1.,0.987688340595138,
1.,0.987688340595138,1.,0.987688340595138,1.,0.987688340595138,1.,0.987688340595138,
1.,0.987688340595138,1.,0.987688340595138,1.,0.987688340595138,1.,0.987688340595138,
1.,0.987688340595138,1.,0.987688340595138,1.,0.987688340595138,1.,0.987688340595138,
1.,0.987688340595138,1.,0.987688340595138,1.,0.987688340595138,1.,0.987688340595138,
1.,0.987688340595138,1.,0.987688340595138,1.,0.987688340595138,1.,0.987688340595138,
1.,0.987688340595138,1.,0.987688340595138,1.,0.987688340595138,1.,0.987688340595138,
1.,0.987688340595138,1.,0.987688340595138,1.,0.987688340595138,1.,0.987688340595138,
1.,0.987688340595138,1.,0.987688340595138,1.,0.987688340595138,1.,0.987688340595138,
1.,0.987688340595138,1.,0.987688340595138,1.,0.987688340595138,1.,0.987688340595138,
1.,0.987688340595138,1.,0.987688340595138,1.,0.987688340595138,1.,0.987688340595138,
1.,0.987688340595138,1.,0.987688340595138,1.,0.987688340595138,1.,0.987688340595138,
1.,0.987688340595138,1.,0.987688340595138,1.,0.987688340595138,1.,0.987688340595138,
1.,0.987688340595138,1.,0.987688340595138,1.,0.987688340595138,1.,0.987688340595138,
1.,0.987688340595138,1.))
REPRESENTATION_ITEM('')
);
#33=(
BOUNDED_CURVE()
B_SPLINE_CURVE(2,(#2460,#2461,#2462,#2463,#2464,#2465,#2466,#2467,#2468,
#2469,#2470,#2471,#2472,#2473,#2474,#2475,#2476,#2477,#2478,#2479,#2480,
#2481,#2482,#2483,#2484,#2485,#2486,#2487,#2488,#2489,#2490,#2491,#2492,
#2493,#2494,#2495,#2496,#2497,#2498,#2499,#2500,#2501,#2502,#2503,#2504,
#2505,#2506,#2507,#2508,#2509,#2510,#2511,#2512,#2513,#2514,#2515,#2516,
#2517,#2518,#2519,#2520,#2521,#2522,#2523,#2524,#2525,#2526,#2527,#2528,
#2529,#2530,#2531,#2532,#2533,#2534,#2535,#2536,#2537,#2538,#2539,#2540,
#2541,#2542,#2543,#2544,#2545,#2546,#2547,#2548,#2549,#2550,#2551,#2552,
#2553,#2554,#2555,#2556,#2557,#2558,#2559,#2560,#2561,#2562,#2563,#2564,
#2565,#2566,#2567,#2568,#2569,#2570,#2571,#2572,#2573,#2574,#2575,#2576,
#2577,#2578,#2579,#2580),.UNSPECIFIED.,.F.,.F.)
B_SPLINE_CURVE_WITH_KNOTS((3,2,2,2,2,2,2,2,2,2,2,2,2,2,2,2,2,2,2,2,2,2,
2,2,2,2,2,2,2,2,2,2,2,2,2,2,2,2,2,2,2,2,2,2,2,2,2,2,2,2,2,2,2,2,2,2,2,2,
2,2,3),(0.,0.0166666666666667,0.0333333333333333,0.05,0.0666666666666667,
0.0833333333333333,0.1,0.116666666666667,0.133333333333333,0.15,0.166666666666667,
0.183333333333333,0.2,0.216666666666667,0.233333333333333,0.25,0.266666666666667,
0.283333333333333,0.3,0.316666666666667,0.333333333333333,0.35,0.366666666666667,
0.383333333333333,0.4,0.416666666666667,0.433333333333333,0.45,0.466666666666667,
0.483333333333333,0.5,0.516666666666667,0.533333333333333,0.55,0.566666666666667,
0.583333333333333,0.6,0.616666666666667,0.633333333333333,0.65,0.666666666666667,
0.683333333333333,0.7,0.716666666666667,0.733333333333333,0.75,0.766666666666667,
0.783333333333333,0.8,0.816666666666667,0.833333333333333,0.85,0.866666666666667,
0.883333333333333,0.9,0.916666666666667,0.933333333333333,0.95,0.966666666666667,
0.983333333333333,1.),.UNSPECIFIED.)
CURVE()
GEOMETRIC_REPRESENTATION_ITEM()
RATIONAL_B_SPLINE_CURVE((1.,0.987688340595138,1.,0.987688340595138,1.,0.987688340595138,
1.,0.987688340595138,1.,0.987688340595138,1.,0.987688340595138,1.,0.987688340595138,
1.,0.987688340595138,1.,0.987688340595138,1.,0.987688340595138,1.,0.987688340595138,
1.,0.987688340595138,1.,0.987688340595138,1.,0.987688340595138,1.,0.987688340595138,
1.,0.987688340595138,1.,0.987688340595138,1.,0.987688340595138,1.,0.987688340595138,
1.,0.987688340595138,1.,0.987688340595138,1.,0.987688340595138,1.,0.987688340595138,
1.,0.987688340595138,1.,0.987688340595138,1.,0.987688340595138,1.,0.987688340595138,
1.,0.987688340595138,1.,0.987688340595138,1.,0.987688340595138,1.,0.987688340595138,
1.,0.987688340595138,1.,0.987688340595138,1.,0.987688340595138,1.,0.987688340595138,
1.,0.987688340595138,1.,0.987688340595138,1.,0.987688340595138,1.,0.987688340595138,
1.,0.987688340595138,1.,0.987688340595138,1.,0.987688340595138,1.,0.987688340595138,
1.,0.987688340595138,1.,0.987688340595138,1.,0.987688340595138,1.,0.987688340595138,
1.,0.987688340595138,1.,0.987688340595138,1.,0.987688340595138,1.,0.987688340595138,
1.,0.987688340595138,1.,0.987688340595138,1.,0.987688340595138,1.,0.987688340595138,
1.,0.987688340595138,1.,0.987688340595138,1.,0.987688340595138,1.,0.987688340595138,
1.,0.987688340595138,1.))
REPRESENTATION_ITEM('')
);
#34=SHAPE_REPRESENTATION_RELATIONSHIP('SRR','None',#2872,#36);
#35=SHAPE_REPRESENTATION_RELATIONSHIP('SRR','None',#2873,#37);
#36=ADVANCED_BREP_SHAPE_REPRESENTATION('',(#40),#2856);
#37=ADVANCED_BREP_SHAPE_REPRESENTATION('',(#41),#2857);
#38=STYLED_ITEM('',(#2890),#40);
#39=STYLED_ITEM('',(#2890),#41);
#40=MANIFOLD_SOLID_BREP('Hopper',#389);
#41=MANIFOLD_SOLID_BREP('Screw Feeder',#390);
#42=CYLINDRICAL_SURFACE('',#423,50.);
#43=CYLINDRICAL_SURFACE('',#425,52.);
#44=CYLINDRICAL_SURFACE('',#429,56.);
#45=CYLINDRICAL_SURFACE('',#435,7.5);
#46=CYLINDRICAL_SURFACE('',#438,7.5);
#47=CYLINDRICAL_SURFACE('',#442,7.5);
#48=CYLINDRICAL_SURFACE('',#445,25.);
#49=LINE('',#569,#72);
#50=LINE('',#574,#73);
#51=LINE('',#578,#74);
#52=LINE('',#583,#75);
#53=LINE('',#590,#76);
#54=LINE('',#598,#77);
#55=LINE('',#644,#78);
#56=LINE('',#660,#79);
#57=LINE('',#1065,#80);
#58=LINE('',#1842,#81);
#59=LINE('',#1843,#82);
#60=LINE('',#1853,#83);
#61=LINE('',#1854,#84);
#62=LINE('',#2828,#85);
#63=LINE('',#2831,#86);
#64=LINE('',#2834,#87);
#65=LINE('',#2836,#88);
#66=LINE('',#2837,#89);
#67=LINE('',#2840,#90);
#68=LINE('',#2842,#91);
#69=LINE('',#2843,#92);
#70=LINE('',#2845,#93);
#71=LINE('',#2846,#94);
#72=VECTOR('',#467,52.);
#73=VECTOR('',#474,200.);
#74=VECTOR('',#479,50.);
#75=VECTOR('',#484,52.);
#76=VECTOR('',#493,56.);
#77=VECTOR('',#504,7.5);
#78=VECTOR('',#505,7.5);
#79=VECTOR('',#514,7.5);
#80=VECTOR('',#517,7.5);
#81=VECTOR('',#524,42.5163970020424);
#82=VECTOR('',#525,3.);
#83=VECTOR('',#528,3.);
#84=VECTOR('',#529,42.5163970020424);
#85=VECTOR('',#534,50.);
#86=VECTOR('',#537,50.);
#87=VECTOR('',#540,8.50510257216822);
#88=VECTOR('',#541,50.);
#89=VECTOR('',#542,8.50510257216822);
#90=VECTOR('',#545,10.);
#91=VECTOR('',#546,50.);
#92=VECTOR('',#547,10.);
#93=VECTOR('',#550,8.50510257216822);
#94=VECTOR('',#551,8.50510257216822);
#95=CONICAL_SURFACE('',#419,52.,0.463647609000806);
#96=CONICAL_SURFACE('',#421,200.,0.463647609000806);
#97=FACE_BOUND('',#127,.T.);
#98=FACE_BOUND('',#133,.T.);
#99=FACE_BOUND('',#136,.T.);
#100=FACE_BOUND('',#138,.T.);
#101=FACE_BOUND('',#153,.T.);
#102=FACE_OUTER_BOUND('',#126,.T.);
#103=FACE_OUTER_BOUND('',#128,.T.);
#104=FACE_OUTER_BOUND('',#129,.T.);
#105=FACE_OUTER_BOUND('',#130,.T.);
#106=FACE_OUTER_BOUND('',#131,.T.);
#107=FACE_OUTER_BOUND('',#132,.T.);
#108=FACE_OUTER_BOUND('',#134,.T.);
#109=FACE_OUTER_BOUND('',#135,.T.);
#110=FACE_OUTER_BOUND('',#137,.T.);
#111=FACE_OUTER_BOUND('',#139,.T.);
#112=FACE_OUTER_BOUND('',#140,.T.);
#113=FACE_OUTER_BOUND('',#141,.T.);
#114=FACE_OUTER_BOUND('',#142,.T.);
#115=FACE_OUTER_BOUND('',#143,.T.);
#116=FACE_OUTER_BOUND('',#144,.T.);
#117=FACE_OUTER_BOUND('',#145,.T.);
#118=FACE_OUTER_BOUND('',#146,.T.);
#119=FACE_OUTER_BOUND('',#147,.T.);
#120=FACE_OUTER_BOUND('',#148,.T.);
#121=FACE_OUTER_BOUND('',#149,.T.);
#122=FACE_OUTER_BOUND('',#150,.T.);
#123=FACE_OUTER_BOUND('',#151,.T.);
#124=FACE_OUTER_BOUND('',#152,.T.);
#125=FACE_OUTER_BOUND('',#154,.T.);
#126=EDGE_LOOP('',(#253));
#127=EDGE_LOOP('',(#254));
#128=EDGE_LOOP('',(#255,#256,#257,#258));
#129=EDGE_LOOP('',(#259,#260,#261,#262));
#130=EDGE_LOOP('',(#263,#264,#265,#266));
#131=EDGE_LOOP('',(#267,#268,#269,#270));
#132=EDGE_LOOP('',(#271));
#133=EDGE_LOOP('',(#272));
#134=EDGE_LOOP('',(#273,#274,#275,#276));
#135=EDGE_LOOP('',(#277));
#136=EDGE_LOOP('',(#278));
#137=EDGE_LOOP('',(#279));
#138=EDGE_LOOP('',(#280));
#139=EDGE_LOOP('',(#281,#282,#283,#284,#285,#286,#287,#288));
#140=EDGE_LOOP('',(#289,#290,#291,#292,#293,#294,#295,#296));
#141=EDGE_LOOP('',(#297));
#142=EDGE_LOOP('',(#298,#299,#300,#301));
#143=EDGE_LOOP('',(#302,#303,#304,#305));
#144=EDGE_LOOP('',(#306,#307,#308,#309));
#145=EDGE_LOOP('',(#310,#311,#312,#313,#314,#315,#316));
#146=EDGE_LOOP('',(#317,#318,#319,#320,#321,#322,#323));
#147=EDGE_LOOP('',(#324,#325,#326,#327));
#148=EDGE_LOOP('',(#328,#329,#330,#331));
#149=EDGE_LOOP('',(#332,#333,#334,#335));
#150=EDGE_LOOP('',(#336,#337,#338,#339));
#151=EDGE_LOOP('',(#340,#341,#342,#343));
#152=EDGE_LOOP('',(#344,#345,#346,#347));
#153=EDGE_LOOP('',(#348));
#154=EDGE_LOOP('',(#349,#350,#351,#352));
#155=CIRCLE('',#417,202.);
#156=CIRCLE('',#418,200.);
#157=CIRCLE('',#420,52.);
#158=CIRCLE('',#422,50.);
#159=CIRCLE('',#424,50.);
#160=CIRCLE('',#426,52.);
#161=CIRCLE('',#427,52.);
#162=CIRCLE('',#430,56.);
#163=CIRCLE('',#431,56.);
#164=CIRCLE('',#436,7.5);
#165=CIRCLE('',#437,1859.05088195134);
#166=CIRCLE('',#439,7.5);
#167=CIRCLE('',#440,1859.05088195135);
#168=CIRCLE('',#446,25.);
#169=CIRCLE('',#447,25.);
#170=VERTEX_POINT('',#563);
#171=VERTEX_POINT('',#565);
#172=VERTEX_POINT('',#568);
#173=VERTEX_POINT('',#572);
#174=VERTEX_POINT('',#576);
#175=VERTEX_POINT('',#580);
#176=VERTEX_POINT('',#582);
#177=VERTEX_POINT('',#587);
#178=VERTEX_POINT('',#589);
#179=VERTEX_POINT('',#596);
#180=VERTEX_POINT('',#597);
#181=VERTEX_POINT('',#599);
#182=VERTEX_POINT('',#643);
#183=VERTEX_POINT('',#646);
#184=VERTEX_POINT('',#650);
#185=VERTEX_POINT('',#657);
#186=VERTEX_POINT('',#659);
#187=VERTEX_POINT('',#661);
#188=VERTEX_POINT('',#1020);
#189=VERTEX_POINT('',#1022);
#190=VERTEX_POINT('',#1064);
#191=VERTEX_POINT('',#1834);
#192=VERTEX_POINT('',#1841);
#193=VERTEX_POINT('',#1845);
#194=VERTEX_POINT('',#1852);
#195=VERTEX_POINT('',#2824);
#196=VERTEX_POINT('',#2825);
#197=VERTEX_POINT('',#2827);
#198=VERTEX_POINT('',#2829);
#199=VERTEX_POINT('',#2833);
#200=VERTEX_POINT('',#2835);
#201=VERTEX_POINT('',#2839);
#202=VERTEX_POINT('',#2841);
#203=EDGE_CURVE('',#170,#170,#155,.T.);
#204=EDGE_CURVE('',#171,#171,#156,.T.);
#205=EDGE_CURVE('',#170,#172,#49,.T.);
#206=EDGE_CURVE('',#172,#172,#157,.T.);
#207=EDGE_CURVE('',#173,#173,#158,.T.);
#208=EDGE_CURVE('',#173,#171,#50,.T.);
#209=EDGE_CURVE('',#174,#174,#159,.F.);
#210=EDGE_CURVE('',#174,#173,#51,.T.);
#211=EDGE_CURVE('',#175,#175,#160,.T.);
#212=EDGE_CURVE('',#175,#176,#52,.T.);
#213=EDGE_CURVE('',#176,#176,#161,.T.);
#214=EDGE_CURVE('',#177,#177,#162,.T.);
#215=EDGE_CURVE('',#177,#178,#53,.T.);
#216=EDGE_CURVE('',#178,#178,#163,.T.);
#217=EDGE_CURVE('',#179,#180,#54,.T.);
#218=EDGE_CURVE('',#181,#179,#28,.T.);
#219=EDGE_CURVE('',#181,#182,#55,.T.);
#220=EDGE_CURVE('',#182,#182,#164,.T.);
#221=EDGE_CURVE('',#183,#181,#29,.T.);
#222=EDGE_CURVE('',#183,#184,#165,.T.);
#223=EDGE_CURVE('',#184,#180,#22,.T.);
#224=EDGE_CURVE('',#185,#185,#166,.T.);
#225=EDGE_CURVE('',#185,#186,#56,.T.);
#226=EDGE_CURVE('',#186,#187,#23,.T.);
#227=EDGE_CURVE('',#187,#188,#167,.T.);
#228=EDGE_CURVE('',#189,#188,#30,.T.);
#229=EDGE_CURVE('',#189,#190,#57,.T.);
#230=EDGE_CURVE('',#190,#186,#24,.T.);
#231=EDGE_CURVE('',#179,#189,#31,.T.);
#232=EDGE_CURVE('',#180,#190,#25,.T.);
#233=EDGE_CURVE('',#184,#191,#26,.T.);
#234=EDGE_CURVE('',#192,#183,#58,.T.);
#235=EDGE_CURVE('',#191,#192,#59,.T.);
#236=EDGE_CURVE('',#193,#187,#27,.T.);
#237=EDGE_CURVE('',#194,#193,#60,.T.);
#238=EDGE_CURVE('',#188,#194,#61,.T.);
#239=EDGE_CURVE('',#191,#193,#32,.T.);
#240=EDGE_CURVE('',#192,#194,#33,.T.);
#241=EDGE_CURVE('',#195,#196,#168,.T.);
#242=EDGE_CURVE('',#197,#196,#62,.T.);
#243=EDGE_CURVE('',#198,#197,#169,.T.);
#244=EDGE_CURVE('',#198,#195,#63,.T.);
#245=EDGE_CURVE('',#196,#199,#64,.T.);
#246=EDGE_CURVE('',#200,#199,#65,.T.);
#247=EDGE_CURVE('',#197,#200,#66,.T.);
#248=EDGE_CURVE('',#199,#201,#67,.T.);
#249=EDGE_CURVE('',#202,#201,#68,.T.);
#250=EDGE_CURVE('',#200,#202,#69,.T.);
#251=EDGE_CURVE('',#201,#195,#70,.T.);
#252=EDGE_CURVE('',#202,#198,#71,.T.);
#253=ORIENTED_EDGE('',*,*,#203,.T.);
#254=ORIENTED_EDGE('',*,*,#204,.F.);
#255=ORIENTED_EDGE('',*,*,#203,.F.);
#256=ORIENTED_EDGE('',*,*,#205,.T.);
#257=ORIENTED_EDGE('',*,*,#206,.F.);
#258=ORIENTED_EDGE('',*,*,#205,.F.);
#259=ORIENTED_EDGE('',*,*,#207,.F.);
#260=ORIENTED_EDGE('',*,*,#208,.T.);
#261=ORIENTED_EDGE('',*,*,#204,.T.);
#262=ORIENTED_EDGE('',*,*,#208,.F.);
#263=ORIENTED_EDGE('',*,*,#209,.F.);
#264=ORIENTED_EDGE('',*,*,#210,.T.);
#265=ORIENTED_EDGE('',*,*,#207,.T.);
#266=ORIENTED_EDGE('',*,*,#210,.F.);
#267=ORIENTED_EDGE('',*,*,#211,.T.);
#268=ORIENTED_EDGE('',*,*,#212,.T.);
#269=ORIENTED_EDGE('',*,*,#213,.F.);
#270=ORIENTED_EDGE('',*,*,#212,.F.);
#271=ORIENTED_EDGE('',*,*,#213,.T.);
#272=ORIENTED_EDGE('',*,*,#209,.T.);
#273=ORIENTED_EDGE('',*,*,#214,.T.);
#274=ORIENTED_EDGE('',*,*,#215,.T.);
#275=ORIENTED_EDGE('',*,*,#216,.F.);
#276=ORIENTED_EDGE('',*,*,#215,.F.);
#277=ORIENTED_EDGE('',*,*,#216,.T.);
#278=ORIENTED_EDGE('',*,*,#211,.F.);
#279=ORIENTED_EDGE('',*,*,#214,.F.);
#280=ORIENTED_EDGE('',*,*,#206,.T.);
#281=ORIENTED_EDGE('',*,*,#217,.F.);
#282=ORIENTED_EDGE('',*,*,#218,.F.);
#283=ORIENTED_EDGE('',*,*,#219,.T.);
#284=ORIENTED_EDGE('',*,*,#220,.F.);
#285=ORIENTED_EDGE('',*,*,#219,.F.);
#286=ORIENTED_EDGE('',*,*,#221,.F.);
#287=ORIENTED_EDGE('',*,*,#222,.T.);
#288=ORIENTED_EDGE('',*,*,#223,.T.);
#289=ORIENTED_EDGE('',*,*,#224,.T.);
#290=ORIENTED_EDGE('',*,*,#225,.T.);
#291=ORIENTED_EDGE('',*,*,#226,.T.);
#292=ORIENTED_EDGE('',*,*,#227,.T.);
#293=ORIENTED_EDGE('',*,*,#228,.F.);
#294=ORIENTED_EDGE('',*,*,#229,.T.);
#295=ORIENTED_EDGE('',*,*,#230,.T.);
#296=ORIENTED_EDGE('',*,*,#225,.F.);
#297=ORIENTED_EDGE('',*,*,#220,.T.);
#298=ORIENTED_EDGE('',*,*,#229,.F.);
#299=ORIENTED_EDGE('',*,*,#231,.F.);
#300=ORIENTED_EDGE('',*,*,#217,.T.);
#301=ORIENTED_EDGE('',*,*,#232,.T.);
#302=ORIENTED_EDGE('',*,*,#233,.F.);
#303=ORIENTED_EDGE('',*,*,#222,.F.);
#304=ORIENTED_EDGE('',*,*,#234,.F.);
#305=ORIENTED_EDGE('',*,*,#235,.F.);
#306=ORIENTED_EDGE('',*,*,#236,.F.);
#307=ORIENTED_EDGE('',*,*,#237,.F.);
#308=ORIENTED_EDGE('',*,*,#238,.F.);
#309=ORIENTED_EDGE('',*,*,#227,.F.);
#310=ORIENTED_EDGE('',*,*,#233,.T.);
#311=ORIENTED_EDGE('',*,*,#239,.T.);
#312=ORIENTED_EDGE('',*,*,#236,.T.);
#313=ORIENTED_EDGE('',*,*,#226,.F.);
#314=ORIENTED_EDGE('',*,*,#230,.F.);
#315=ORIENTED_EDGE('',*,*,#232,.F.);
#316=ORIENTED_EDGE('',*,*,#223,.F.);
#317=ORIENTED_EDGE('',*,*,#234,.T.);
#318=ORIENTED_EDGE('',*,*,#221,.T.);
#319=ORIENTED_EDGE('',*,*,#218,.T.);
#320=ORIENTED_EDGE('',*,*,#231,.T.);
#321=ORIENTED_EDGE('',*,*,#228,.T.);
#322=ORIENTED_EDGE('',*,*,#238,.T.);
#323=ORIENTED_EDGE('',*,*,#240,.F.);
#324=ORIENTED_EDGE('',*,*,#235,.T.);
#325=ORIENTED_EDGE('',*,*,#240,.T.);
#326=ORIENTED_EDGE('',*,*,#237,.T.);
#327=ORIENTED_EDGE('',*,*,#239,.F.);
#328=ORIENTED_EDGE('',*,*,#241,.T.);
#329=ORIENTED_EDGE('',*,*,#242,.F.);
#330=ORIENTED_EDGE('',*,*,#243,.F.);
#331=ORIENTED_EDGE('',*,*,#244,.T.);
#332=ORIENTED_EDGE('',*,*,#245,.T.);
#333=ORIENTED_EDGE('',*,*,#246,.F.);
#334=ORIENTED_EDGE('',*,*,#247,.F.);
#335=ORIENTED_EDGE('',*,*,#242,.T.);
#336=ORIENTED_EDGE('',*,*,#248,.T.);
#337=ORIENTED_EDGE('',*,*,#249,.F.);
#338=ORIENTED_EDGE('',*,*,#250,.F.);
#339=ORIENTED_EDGE('',*,*,#246,.T.);
#340=ORIENTED_EDGE('',*,*,#251,.T.);
#341=ORIENTED_EDGE('',*,*,#244,.F.);
#342=ORIENTED_EDGE('',*,*,#252,.F.);
#343=ORIENTED_EDGE('',*,*,#249,.T.);
#344=ORIENTED_EDGE('',*,*,#243,.T.);
#345=ORIENTED_EDGE('',*,*,#247,.T.);
#346=ORIENTED_EDGE('',*,*,#250,.T.);
#347=ORIENTED_EDGE('',*,*,#252,.T.);
#348=ORIENTED_EDGE('',*,*,#224,.F.);
#349=ORIENTED_EDGE('',*,*,#241,.F.);
#350=ORIENTED_EDGE('',*,*,#251,.F.);
#351=ORIENTED_EDGE('',*,*,#248,.F.);
#352=ORIENTED_EDGE('',*,*,#245,.F.);
#353=PLANE('',#416);
#354=PLANE('',#428);
#355=PLANE('',#432);
#356=PLANE('',#433);
#357=PLANE('',#441);
#358=PLANE('',#443);
#359=PLANE('',#444);
#360=PLANE('',#448);
#361=PLANE('',#449);
#362=PLANE('',#450);
#363=PLANE('',#451);
#364=PLANE('',#452);
#365=ADVANCED_FACE('',(#102,#97),#353,.F.);
#366=ADVANCED_FACE('',(#103),#95,.T.);
#367=ADVANCED_FACE('',(#104),#96,.F.);
#368=ADVANCED_FACE('',(#105),#42,.F.);
#369=ADVANCED_FACE('',(#106),#43,.T.);
#370=ADVANCED_FACE('',(#107,#98),#354,.T.);
#371=ADVANCED_FACE('',(#108),#44,.T.);
#372=ADVANCED_FACE('',(#109,#99),#355,.T.);
#373=ADVANCED_FACE('',(#110,#100),#356,.F.);
#374=ADVANCED_FACE('',(#111),#45,.T.);
#375=ADVANCED_FACE('',(#112),#46,.T.);
#376=ADVANCED_FACE('',(#113),#357,.T.);
#377=ADVANCED_FACE('',(#114),#47,.T.);
#378=ADVANCED_FACE('',(#115),#358,.F.);
#379=ADVANCED_FACE('',(#116),#359,.F.);
#380=ADVANCED_FACE('',(#117),#19,.T.);
#381=ADVANCED_FACE('',(#118),#20,.T.);
#382=ADVANCED_FACE('',(#119),#21,.T.);
#383=ADVANCED_FACE('',(#120),#48,.T.);
#384=ADVANCED_FACE('',(#121),#360,.F.);
#385=ADVANCED_FACE('',(#122),#361,.F.);
#386=ADVANCED_FACE('',(#123),#362,.F.);
#387=ADVANCED_FACE('',(#124,#101),#363,.T.);
#388=ADVANCED_FACE('',(#125),#364,.F.);
#389=CLOSED_SHELL('',(#365,#366,#367,#368,#369,#370,#371,#372,#373));
#390=CLOSED_SHELL('',(#374,#375,#376,#377,#378,#379,#380,#381,#382,#383,
#384,#385,#386,#387,#388));
#391=DERIVED_UNIT_ELEMENT(#395,1.);
#392=DERIVED_UNIT_ELEMENT(#2860,-3.);
#393=DERIVED_UNIT_ELEMENT(#395,1.);
#394=DERIVED_UNIT_ELEMENT(#2860,-3.);
#395=(
MASS_UNIT()
NAMED_UNIT(*)
SI_UNIT(.KILO.,.GRAM.)
);
#396=DERIVED_UNIT((#391,#392));
#397=DERIVED_UNIT((#393,#394));
#398=MEASURE_REPRESENTATION_ITEM('density measure',
POSITIVE_RATIO_MEASURE(7850.),#396);
#399=MEASURE_REPRESENTATION_ITEM('density measure',
POSITIVE_RATIO_MEASURE(7850.),#397);
#400=PROPERTY_DEFINITION_REPRESENTATION(#410,#404);
#401=PROPERTY_DEFINITION_REPRESENTATION(#411,#405);
#402=PROPERTY_DEFINITION_REPRESENTATION(#412,#406);
#403=PROPERTY_DEFINITION_REPRESENTATION(#413,#407);
#404=REPRESENTATION('material name',(#408),#2856);
#405=REPRESENTATION('density',(#398),#2856);
#406=REPRESENTATION('material name',(#409),#2857);
#407=REPRESENTATION('density',(#399),#2857);
#408=DESCRIPTIVE_REPRESENTATION_ITEM('Steel','Steel');
#409=DESCRIPTIVE_REPRESENTATION_ITEM('Steel','Steel');
#410=PROPERTY_DEFINITION('material property','material name',#2876);
#411=PROPERTY_DEFINITION('material property','density of part',#2876);
#412=PROPERTY_DEFINITION('material property','material name',#2877);
#413=PROPERTY_DEFINITION('material property','density of part',#2877);
#414=AXIS2_PLACEMENT_3D('',#560,#455,#456);
#415=AXIS2_PLACEMENT_3D('',#561,#457,#458);
#416=AXIS2_PLACEMENT_3D('',#562,#459,#460);
#417=AXIS2_PLACEMENT_3D('',#564,#461,#462);
#418=AXIS2_PLACEMENT_3D('',#566,#463,#464);
#419=AXIS2_PLACEMENT_3D('',#567,#465,#466);
#420=AXIS2_PLACEMENT_3D('',#570,#468,#469);
#421=AXIS2_PLACEMENT_3D('',#571,#470,#471);
#422=AXIS2_PLACEMENT_3D('',#573,#472,#473);
#423=AXIS2_PLACEMENT_3D('',#575,#475,#476);
#424=AXIS2_PLACEMENT_3D('',#577,#477,#478);
#425=AXIS2_PLACEMENT_3D('',#579,#480,#481);
#426=AXIS2_PLACEMENT_3D('',#581,#482,#483);
#427=AXIS2_PLACEMENT_3D('',#584,#485,#486);
#428=AXIS2_PLACEMENT_3D('',#585,#487,#488);
#429=AXIS2_PLACEMENT_3D('',#586,#489,#490);
#430=AXIS2_PLACEMENT_3D('',#588,#491,#492);
#431=AXIS2_PLACEMENT_3D('',#591,#494,#495);
#432=AXIS2_PLACEMENT_3D('',#592,#496,#497);
#433=AXIS2_PLACEMENT_3D('',#593,#498,#499);
#434=AXIS2_PLACEMENT_3D('',#594,#500,#501);
#435=AXIS2_PLACEMENT_3D('',#595,#502,#503);
#436=AXIS2_PLACEMENT_3D('',#645,#506,#507);
#437=AXIS2_PLACEMENT_3D('',#651,#508,#509);
#438=AXIS2_PLACEMENT_3D('',#656,#510,#511);
#439=AXIS2_PLACEMENT_3D('',#658,#512,#513);
#440=AXIS2_PLACEMENT_3D('',#1021,#515,#516);
#441=AXIS2_PLACEMENT_3D('',#1427,#518,#519);
#442=AXIS2_PLACEMENT_3D('',#1428,#520,#521);
#443=AXIS2_PLACEMENT_3D('',#1833,#522,#523);
#444=AXIS2_PLACEMENT_3D('',#1844,#526,#527);
#445=AXIS2_PLACEMENT_3D('',#2823,#530,#531);
#446=AXIS2_PLACEMENT_3D('',#2826,#532,#533);
#447=AXIS2_PLACEMENT_3D('',#2830,#535,#536);
#448=AXIS2_PLACEMENT_3D('',#2832,#538,#539);
#449=AXIS2_PLACEMENT_3D('',#2838,#543,#544);
#450=AXIS2_PLACEMENT_3D('',#2844,#548,#549);
#451=AXIS2_PLACEMENT_3D('',#2847,#552,#553);
#452=AXIS2_PLACEMENT_3D('',#2848,#554,#555);
#453=AXIS2_PLACEMENT_3D('',#2849,#556,#557);
#454=AXIS2_PLACEMENT_3D('',#2850,#558,#559);
#455=DIRECTION('axis',(0.,0.,1.));
#456=DIRECTION('refdir',(1.,0.,0.));
#457=DIRECTION('axis',(0.,0.,1.));
#458=DIRECTION('refdir',(1.,0.,0.));
#459=DIRECTION('center_axis',(0.,-1.,0.));
#460=DIRECTION('ref_axis',(0.,0.,-1.));
#461=DIRECTION('center_axis',(0.,1.,0.));
#462=DIRECTION('ref_axis',(0.,0.,1.));
#463=DIRECTION('center_axis',(0.,1.,0.));
#464=DIRECTION('ref_axis',(0.,0.,1.));
#465=DIRECTION('center_axis',(0.,1.,0.));
#466=DIRECTION('ref_axis',(0.,0.,1.));
#467=DIRECTION('',(5.47678698264202E-17,-0.894427190999916,0.447213595499958));
#468=DIRECTION('center_axis',(0.,-1.,0.));
#469=DIRECTION('ref_axis',(0.,0.,-1.));
#470=DIRECTION('center_axis',(0.,1.,0.));
#471=DIRECTION('ref_axis',(0.,0.,1.));
#472=DIRECTION('center_axis',(0.,1.,0.));
#473=DIRECTION('ref_axis',(0.,0.,1.));
#474=DIRECTION('',(-5.47678698264202E-17,0.894427190999916,-0.447213595499958));
#475=DIRECTION('center_axis',(0.,1.,0.));
#476=DIRECTION('ref_axis',(0.,0.,1.));
#477=DIRECTION('center_axis',(0.,-1.,0.));
#478=DIRECTION('ref_axis',(0.,0.,-1.));
#479=DIRECTION('',(0.,1.,0.));
#480=DIRECTION('center_axis',(0.,1.,0.));
#481=DIRECTION('ref_axis',(0.,0.,1.));
#482=DIRECTION('center_axis',(0.,-1.,0.));
#483=DIRECTION('ref_axis',(0.,0.,-1.));
#484=DIRECTION('',(0.,-1.,0.));
#485=DIRECTION('center_axis',(0.,-1.,0.));
#486=DIRECTION('ref_axis',(0.,0.,-1.));
#487=DIRECTION('center_axis',(0.,-1.,0.));
#488=DIRECTION('ref_axis',(0.,0.,-1.));
#489=DIRECTION('center_axis',(0.,1.,0.));
#490=DIRECTION('ref_axis',(0.,0.,1.));
#491=DIRECTION('center_axis',(0.,-1.,0.));
#492=DIRECTION('ref_axis',(0.,0.,-1.));
#493=DIRECTION('',(0.,-1.,0.));
#494=DIRECTION('center_axis',(0.,-1.,0.));
#495=DIRECTION('ref_axis',(0.,0.,-1.));
#496=DIRECTION('center_axis',(0.,-1.,0.));
#497=DIRECTION('ref_axis',(0.,0.,-1.));
#498=DIRECTION('center_axis',(0.,-1.,0.));
#499=DIRECTION('ref_axis',(0.,0.,-1.));
#500=DIRECTION('axis',(0.,0.,1.));
#501=DIRECTION('refdir',(1.,0.,0.));
#502=DIRECTION('center_axis',(0.,-1.,0.));
#503=DIRECTION('ref_axis',(0.,0.,-1.));
#504=DIRECTION('',(0.,1.,0.));
#505=DIRECTION('',(0.,1.,0.));
#506=DIRECTION('center_axis',(0.,1.,0.));
#507=DIRECTION('ref_axis',(-0.715662544779069,0.,-0.698446219833959));
#508=DIRECTION('center_axis',(0.997979715186782,0.0635333619109602,1.57664132857237E-12));
#509=DIRECTION('ref_axis',(0.000102666233862281,-0.00161267745569481,0.999998694364682));
#510=DIRECTION('center_axis',(0.,-1.,0.));
#511=DIRECTION('ref_axis',(0.,0.,-1.));
#512=DIRECTION('center_axis',(0.,1.,0.));
#513=DIRECTION('ref_axis',(0.,0.,1.));
#514=DIRECTION('',(0.,1.,0.));
#515=DIRECTION('center_axis',(-0.997979715186782,-0.0635333619109597,-1.60052983355074E-12));
#516=DIRECTION('ref_axis',(1.40886995536597E-7,-2.21307290245903E-6,0.999999999997541));
#517=DIRECTION('',(0.,1.,0.));
#518=DIRECTION('center_axis',(0.,1.,0.));
#519=DIRECTION('ref_axis',(-0.715662544779069,0.,-0.698446219833959));
#520=DIRECTION('center_axis',(0.,-1.,0.));
#521=DIRECTION('ref_axis',(0.,0.,-1.));
#522=DIRECTION('center_axis',(-0.997979715186782,-0.0635333619109615,0.));
#523=DIRECTION('ref_axis',(0.,0.,1.));
#524=DIRECTION('',(7.77774425693207E-18,0.,-1.));
#525=DIRECTION('',(-0.0635333619109615,0.997979715186782,0.));
#526=DIRECTION('center_axis',(0.997979715186782,0.063533361910961,0.));
#527=DIRECTION('ref_axis',(0.,0.,-1.));
#528=DIRECTION('',(0.0635333619109615,-0.997979715186782,0.));
#529=DIRECTION('',(-7.77774425693207E-18,0.,1.));
#530=DIRECTION('center_axis',(0.,-1.,0.));
#531=DIRECTION('ref_axis',(-3.21624529935327E-16,0.,1.));
#532=DIRECTION('center_axis',(0.,1.,0.));
#533=DIRECTION('ref_axis',(0.,0.,1.));
#534=DIRECTION('',(0.,-1.,0.));
#535=DIRECTION('center_axis',(0.,1.,0.));
#536=DIRECTION('ref_axis',(0.,0.,1.));
#537=DIRECTION('',(0.,-1.,0.));
#538=DIRECTION('center_axis',(-1.,0.,-4.07925350989523E-16));
#539=DIRECTION('ref_axis',(-4.07925350989523E-16,0.,1.));
#540=DIRECTION('',(3.91608336949942E-16,0.,-1.));
#541=DIRECTION('',(0.,-1.,0.));
#542=DIRECTION('',(3.91608336949942E-16,0.,-1.));
#543=DIRECTION('center_axis',(0.,0.,1.));
#544=DIRECTION('ref_axis',(1.,0.,0.));
#545=DIRECTION('',(-1.,0.,0.));
#546=DIRECTION('',(0.,-1.,0.));
#547=DIRECTION('',(-1.,0.,0.));
#548=DIRECTION('center_axis',(1.,0.,-4.07925350989523E-16));
#549=DIRECTION('ref_axis',(-4.07925350989523E-16,0.,-1.));
#550=DIRECTION('',(3.91608336949942E-16,0.,1.));
#551=DIRECTION('',(3.91608336949942E-16,0.,1.));
#552=DIRECTION('center_axis',(0.,1.,0.));
#553=DIRECTION('ref_axis',(0.,0.,1.));
#554=DIRECTION('center_axis',(0.,1.,0.));
#555=DIRECTION('ref_axis',(0.,0.,1.));
#556=DIRECTION('',(-0.012051316852849,0.,0.999927380244242));
#557=DIRECTION('',(0.999927380244242,0.,0.012051316852849));
#558=DIRECTION('',(0.698446233568507,0.,0.715662531374926));
#559=DIRECTION('',(0.715662531374926,0.,-0.698446233568507));
#560=CARTESIAN_POINT('',(0.,0.,0.));
#561=CARTESIAN_POINT('',(0.,0.,0.));
#562=CARTESIAN_POINT('Origin',(200.,150.,0.));
#563=CARTESIAN_POINT('',(-2.47378653427765E-14,150.,-202.));
#564=CARTESIAN_POINT('Origin',(0.,150.,0.));
#565=CARTESIAN_POINT('',(-2.44929359829471E-14,150.,-200.));
#566=CARTESIAN_POINT('Origin',(0.,150.,0.));
#567=CARTESIAN_POINT('Origin',(0.,-150.,0.));
#568=CARTESIAN_POINT('',(0.,-150.,-52.));
#569=CARTESIAN_POINT('',(-6.36816335556624E-15,-150.,-52.));
#570=CARTESIAN_POINT('Origin',(0.,-150.,0.));
#571=CARTESIAN_POINT('Origin',(0.,150.,0.));
#572=CARTESIAN_POINT('',(-6.12323399573677E-15,-150.,-50.0000000000001));
#573=CARTESIAN_POINT('Origin',(0.,-150.,0.));
#574=CARTESIAN_POINT('',(-2.44929359829471E-14,150.,-200.));
#575=CARTESIAN_POINT('Origin',(0.,-170.,0.));
#576=CARTESIAN_POINT('',(0.,-170.,-50.));
#577=CARTESIAN_POINT('Origin',(0.,-170.,0.));
#578=CARTESIAN_POINT('',(-6.12323399573677E-15,-170.,-50.));
#579=CARTESIAN_POINT('Origin',(0.,-170.,0.));
#580=CARTESIAN_POINT('',(0.,-152.,-52.));
#581=CARTESIAN_POINT('Origin',(0.,-152.,0.));
#582=CARTESIAN_POINT('',(0.,-170.,-52.));
#583=CARTESIAN_POINT('',(-6.36816335556624E-15,-170.,-52.));
#584=CARTESIAN_POINT('Origin',(0.,-170.,0.));
#585=CARTESIAN_POINT('Origin',(0.,-170.,0.));
#586=CARTESIAN_POINT('Origin',(0.,-152.,0.));
#587=CARTESIAN_POINT('',(0.,-150.,-56.));
#588=CARTESIAN_POINT('Origin',(0.,-150.,0.));
#589=CARTESIAN_POINT('',(0.,-152.,-56.));
#590=CARTESIAN_POINT('',(-6.85802207522518E-15,-152.,-56.));
#591=CARTESIAN_POINT('Origin',(0.,-152.,0.));
#592=CARTESIAN_POINT('Origin',(0.,-152.,0.));
#593=CARTESIAN_POINT('Origin',(0.,-150.,0.));
#594=CARTESIAN_POINT('',(0.,0.,0.));
#595=CARTESIAN_POINT('Origin',(0.,240.,0.));
#596=CARTESIAN_POINT('',(-1.90241102001116E-16,217.99585953923,7.50000000439337));
#597=CARTESIAN_POINT('',(-4.06843950140785E-7,234.921557632927,7.50242802810186));
#598=CARTESIAN_POINT('',(-9.18485099360515E-16,240.,7.5));
#599=CARTESIAN_POINT('',(-9.18479639923619E-16,237.99585953923,7.50000000439337));
#600=CARTESIAN_POINT('Ctrl Pts',(-9.1847417994869E-16,237.99585953923,7.50000000439337));
#601=CARTESIAN_POINT('Ctrl Pts',(-1.18775172812193,237.495912211348,7.50000000439337));
#602=CARTESIAN_POINT('Ctrl Pts',(-2.317383311169,236.995967593475,7.13300320026677));
#603=CARTESIAN_POINT('Ctrl Pts',(-3.44714003087638,236.495967593475,6.76596574150984));
#604=CARTESIAN_POINT('Ctrl Pts',(-4.40818170865423,235.995967593475,6.06777834873578));
#605=CARTESIAN_POINT('Ctrl Pts',(-5.36922338643209,235.495967593475,5.36959095596173));
#606=CARTESIAN_POINT('Ctrl Pts',(-6.06747656688843,234.995967593475,4.40859707573286));
#607=CARTESIAN_POINT('Ctrl Pts',(-6.76572974734476,234.495967593475,3.447603195504));
#608=CARTESIAN_POINT('Ctrl Pts',(-7.13284454416054,233.995967593475,2.31787160445521));
#609=CARTESIAN_POINT('Ctrl Pts',(-7.49995934097631,233.495967593475,1.18814001340642));
#610=CARTESIAN_POINT('Ctrl Pts',(-7.5,232.995967593475,0.000256710972401669));
#611=CARTESIAN_POINT('Ctrl Pts',(-7.50004065902369,232.495967593475,-1.18762659146162));
#612=CARTESIAN_POINT('Ctrl Pts',(-7.13300320026677,231.995967593475,-2.317383311169));
#613=CARTESIAN_POINT('Ctrl Pts',(-6.76596574150984,231.495967593475,-3.44714003087638));
#614=CARTESIAN_POINT('Ctrl Pts',(-6.06777834873578,230.995967593475,-4.40818170865423));
#615=CARTESIAN_POINT('Ctrl Pts',(-5.36959095596173,230.495967593475,-5.36922338643209));
#616=CARTESIAN_POINT('Ctrl Pts',(-4.40859707573286,229.995967593475,-6.06747656688843));
#617=CARTESIAN_POINT('Ctrl Pts',(-3.447603195504,229.495967593475,-6.76572974734476));
#618=CARTESIAN_POINT('Ctrl Pts',(-2.31787160445521,228.995967593475,-7.13284454416054));
#619=CARTESIAN_POINT('Ctrl Pts',(-1.18814001340642,228.495967593475,-7.49995934097631));
#620=CARTESIAN_POINT('Ctrl Pts',(-0.000256710972402128,227.995967593475,
-7.5));
#621=CARTESIAN_POINT('Ctrl Pts',(1.18762659146162,227.495967593475,-7.50004065902369));
#622=CARTESIAN_POINT('Ctrl Pts',(2.317383311169,226.995967593475,-7.13300320026677));
#623=CARTESIAN_POINT('Ctrl Pts',(3.44714003087638,226.495967593475,-6.76596574150984));
#624=CARTESIAN_POINT('Ctrl Pts',(4.40818170865423,225.995967593475,-6.06777834873578));
#625=CARTESIAN_POINT('Ctrl Pts',(5.36922338643209,225.495967593475,-5.36959095596173));
#626=CARTESIAN_POINT('Ctrl Pts',(6.06747656688843,224.995967593475,-4.40859707573286));
#627=CARTESIAN_POINT('Ctrl Pts',(6.76572974734476,224.495967593475,-3.447603195504));
#628=CARTESIAN_POINT('Ctrl Pts',(7.13284454416054,223.995967593475,-2.31787160445521));
#629=CARTESIAN_POINT('Ctrl Pts',(7.49995934097631,223.495967593475,-1.18814001340642));
#630=CARTESIAN_POINT('Ctrl Pts',(7.5,222.995967593475,-0.000256710972402588));
#631=CARTESIAN_POINT('Ctrl Pts',(7.50004065902369,222.495967593475,1.18762659146162));
#632=CARTESIAN_POINT('Ctrl Pts',(7.13300320026677,221.995967593475,2.317383311169));
#633=CARTESIAN_POINT('Ctrl Pts',(6.76596574150984,221.495967593475,3.44714003087638));
#634=CARTESIAN_POINT('Ctrl Pts',(6.06777834873579,220.995967593475,4.40818170865423));
#635=CARTESIAN_POINT('Ctrl Pts',(5.36959095596173,220.495967593475,5.36922338643209));
#636=CARTESIAN_POINT('Ctrl Pts',(4.40859707573286,219.995967593475,6.06747656688843));
#637=CARTESIAN_POINT('Ctrl Pts',(3.447603195504,219.495967593475,6.76572974734476));
#638=CARTESIAN_POINT('Ctrl Pts',(2.31787160445521,218.995967593475,7.13284454416054));
#639=CARTESIAN_POINT('Ctrl Pts',(1.18814001340643,218.495967593475,7.49995934097631));
#640=CARTESIAN_POINT('Ctrl Pts',(0.00025671097240121,217.995967593475,7.5));
#641=CARTESIAN_POINT('Ctrl Pts',(0.000128355486249734,217.995913566499,
7.50000000439337));
#642=CARTESIAN_POINT('Ctrl Pts',(5.38002895896315E-16,217.99585953923,7.50000000439337));
#643=CARTESIAN_POINT('',(-9.18485099360515E-16,400.,7.5));
#644=CARTESIAN_POINT('',(-9.18485099360515E-16,240.,7.5));
#645=CARTESIAN_POINT('Origin',(0.,400.,3.5527136788005E-14));
#646=CARTESIAN_POINT('',(0.00025671099249169,237.995967593476,7.49999999788428));
#647=CARTESIAN_POINT('Ctrl Pts',(0.00025671097240121,237.995967593475,7.5));
#648=CARTESIAN_POINT('Ctrl Pts',(0.000128355486236195,237.995913566499,
7.50000000439337));
#649=CARTESIAN_POINT('Ctrl Pts',(-9.1847417994869E-16,237.99585953923,7.50000000439337));
#650=CARTESIAN_POINT('',(0.19085679599498,235.002028447937,7.49999995822451));
#651=CARTESIAN_POINT('Origin',(-5.20522648770767E-6,238.000081810591,-1851.55088195117));
#652=CARTESIAN_POINT('Ctrl Pts',(0.190856796705285,235.002028447915,7.5));
#653=CARTESIAN_POINT('Ctrl Pts',(0.127311648028415,234.975281229334,7.50161706980302));
#654=CARTESIAN_POINT('Ctrl Pts',(0.0636823578853783,234.948453397593,7.50242803155527));
#655=CARTESIAN_POINT('Ctrl Pts',(-4.06843934450864E-7,234.921557632927,
7.50242802810186));
#656=CARTESIAN_POINT('Origin',(0.,240.,0.));
#657=CARTESIAN_POINT('',(0.,150.,7.5));
#658=CARTESIAN_POINT('Origin',(0.,150.,0.));
#659=CARTESIAN_POINT('',(-4.0684396522591E-7,194.921557632927,7.50242802810186));
#660=CARTESIAN_POINT('',(-9.18485099360515E-16,240.,7.5));
#661=CARTESIAN_POINT('',(0.190870214476193,175.002034095778,7.4999996458277));
#662=CARTESIAN_POINT('Ctrl Pts',(-4.06843965232862E-7,194.921557632927,
7.50242802810186));
#663=CARTESIAN_POINT('Ctrl Pts',(-0.152090385415712,194.857323985265,7.50242801985428));
#664=CARTESIAN_POINT('Ctrl Pts',(-0.304485788637936,194.792702491972,7.49779895914529));
#665=CARTESIAN_POINT('Ctrl Pts',(-0.456762644214526,194.727870534021,7.48851081348613));
#666=CARTESIAN_POINT('Ctrl Pts',(-0.609070650330248,194.663025313709,7.47922076779598));
#667=CARTESIAN_POINT('Ctrl Pts',(-0.761259533137463,194.597969762789,7.46526968655078));
#668=CARTESIAN_POINT('Ctrl Pts',(-0.91290272043789,194.532885263598,7.44667945730617));
#669=CARTESIAN_POINT('Ctrl Pts',(-1.06450493068591,194.467818351553,7.42809425151703));
#670=CARTESIAN_POINT('Ctrl Pts',(-1.2155612127976,194.402722732839,7.40487246128588));
#671=CARTESIAN_POINT('Ctrl Pts',(-1.36565093134532,194.337780178401,7.37708776215684));
#672=CARTESIAN_POINT('Ctrl Pts',(-1.51579830432436,194.272812677376,7.34929239000474));
#673=CARTESIAN_POINT('Ctrl Pts',(-1.6649778616245,194.207998581557,7.31693074896081));
#674=CARTESIAN_POINT('Ctrl Pts',(-1.81278187771196,194.143517028959,7.28012693438018));
#675=CARTESIAN_POINT('Ctrl Pts',(-1.92135204017681,194.096151789321,7.25309251248746));
#676=CARTESIAN_POINT('Ctrl Pts',(-2.02918025203168,194.04896593395,7.22366229239575));
#677=CARTESIAN_POINT('Ctrl Pts',(-2.13611185762632,194.002028447915,7.19190186588755));
#678=CARTESIAN_POINT('Ctrl Pts',(-2.2816613117044,193.938139708658,7.14867131011455));
#679=CARTESIAN_POINT('Ctrl Pts',(-2.42624566734731,193.87379055128,7.10091475754277));
#680=CARTESIAN_POINT('Ctrl Pts',(-2.56944875671864,193.809155844927,7.04871331545309));
#681=CARTESIAN_POINT('Ctrl Pts',(-2.71813540129491,193.74204613624,6.99451296753858));
#682=CARTESIAN_POINT('Ctrl Pts',(-2.86533230206808,193.674628800623,6.93552054364116));
#683=CARTESIAN_POINT('Ctrl Pts',(-3.01058579312346,193.607105531561,6.87188471229631));
#684=CARTESIAN_POINT('Ctrl Pts',(-3.15046347852857,193.542081286575,6.81060403165537));
#685=CARTESIAN_POINT('Ctrl Pts',(-3.28853853492898,193.476959054234,6.74501779444794));
#686=CARTESIAN_POINT('Ctrl Pts',(-3.42442461876489,193.411920847683,6.67530840839924));
#687=CARTESIAN_POINT('Ctrl Pts',(-3.5602870648691,193.346893954694,6.60561114847646));
#688=CARTESIAN_POINT('Ctrl Pts',(-3.693960843474,193.281951283189,6.53179244342482));
#689=CARTESIAN_POINT('Ctrl Pts',(-3.82508551083643,193.217273190526,6.45407988420021));
#690=CARTESIAN_POINT('Ctrl Pts',(-3.95624536474471,193.152577741872,6.37634647125995));
#691=CARTESIAN_POINT('Ctrl Pts',(-4.0848543388159,193.088147231022,6.2947174573996));
#692=CARTESIAN_POINT('Ctrl Pts',(-4.21058385833655,193.024157275819,6.20946132033724));
#693=CARTESIAN_POINT('Ctrl Pts',(-4.22508868089454,193.016775056041,6.1996257213086));
#694=CARTESIAN_POINT('Ctrl Pts',(-4.23955521930311,193.009398692253,6.18974188939153));
#695=CARTESIAN_POINT('Ctrl Pts',(-4.25398300016701,193.002028447915,6.17981026821526));
#696=CARTESIAN_POINT('Ctrl Pts',(-4.37904978050105,192.938139708658,6.09371831161215));
#697=CARTESIAN_POINT('Ctrl Pts',(-4.50180008775214,192.87379055128,6.00362010807856));
#698=CARTESIAN_POINT('Ctrl Pts',(-4.62186318631576,192.809155844927,5.90972139815641));
#699=CARTESIAN_POINT('Ctrl Pts',(-4.74652375991947,192.74204613624,5.8122271040762));
#700=CARTESIAN_POINT('Ctrl Pts',(-4.86828667005456,192.674628800622,5.71063563105828));
#701=CARTESIAN_POINT('Ctrl Pts',(-4.98676639590067,192.607105531561,5.6052285617595));
#702=CARTESIAN_POINT('Ctrl Pts',(-5.10086120834454,192.542081286575,5.50372258918893));
#703=CARTESIAN_POINT('Ctrl Pts',(-5.21191112857775,192.476959054234,5.39867883198654));
#704=CARTESIAN_POINT('Ctrl Pts',(-5.31960508912721,192.411920847683,5.29039015693365));
#705=CARTESIAN_POINT('Ctrl Pts',(-5.42728031603782,192.346893954693,5.18212031897172));
#706=CARTESIAN_POINT('Ctrl Pts',(-5.53160039987492,192.281951283188,5.07060708921572));
#707=CARTESIAN_POINT('Ctrl Pts',(-5.632292867741,192.217273190525,4.95617830276943));
#708=CARTESIAN_POINT('Ctrl Pts',(-5.73301235584602,192.152577741871,4.84171881002288));
#709=CARTESIAN_POINT('Ctrl Pts',(-5.83010200617219,192.088147231023,4.72434264585674));
#710=CARTESIAN_POINT('Ctrl Pts',(-5.92333228977468,192.02415727582,4.60440668292466));
#711=CARTESIAN_POINT('Ctrl Pts',(-5.93408782853699,192.016775056042,4.59057023570531));
#712=CARTESIAN_POINT('Ctrl Pts',(-5.94479205212731,192.009398692253,4.5766997467359));
#713=CARTESIAN_POINT('Ctrl Pts',(-5.95544464740897,192.002028447915,4.56279578422008));
#714=CARTESIAN_POINT('Ctrl Pts',(-6.04778634614874,191.938139708657,4.44226970733661));
#715=CARTESIAN_POINT('Ctrl Pts',(-6.13668694968295,191.87379055128,4.31864929275364));
#716=CARTESIAN_POINT('Ctrl Pts',(-6.22185744482296,191.809155844926,4.19224477495645));
#717=CARTESIAN_POINT('Ctrl Pts',(-6.31028930194836,191.742046136239,4.0609999554979));
#718=CARTESIAN_POINT('Ctrl Pts',(-6.39469921942917,191.674628800622,3.92675391456802));
#719=CARTESIAN_POINT('Ctrl Pts',(-6.47480755900329,191.60710553156,3.78989358567263));
#720=CARTESIAN_POINT('Ctrl Pts',(-6.55195110329862,191.542081286575,3.65809843300132));
#721=CARTESIAN_POINT('Ctrl Pts',(-6.6251055474419,191.476959054234,3.5238795706418));
#722=CARTESIAN_POINT('Ctrl Pts',(-6.69406554949839,191.411920847682,3.38761165659044));
#723=CARTESIAN_POINT('Ctrl Pts',(-6.76301355578597,191.346893954693,3.2513674466916));
#724=CARTESIAN_POINT('Ctrl Pts',(-6.82776836820671,191.281951283189,3.11307538412042));
#725=CARTESIAN_POINT('Ctrl Pts',(-6.88817215625433,191.217273190527,2.97313145734446));
#726=CARTESIAN_POINT('Ctrl Pts',(-6.94859215330858,191.152577741872,2.83314997742638));
#727=CARTESIAN_POINT('Ctrl Pts',(-7.00465866845448,191.088147231024,2.69151625970926));
#728=CARTESIAN_POINT('Ctrl Pts',(-7.05626368640816,191.024157275821,2.54864063860052));
#729=CARTESIAN_POINT('Ctrl Pts',(-7.06221711430205,191.016775056042,2.53215775104821));
#730=CARTESIAN_POINT('Ctrl Pts',(-7.06811121908795,191.009398692254,2.51565834512789));
#731=CARTESIAN_POINT('Ctrl Pts',(-7.07394587853975,191.002028447915,2.49914305799789));
#732=CARTESIAN_POINT('Ctrl Pts',(-7.12452344682944,190.938139708658,2.35598079299494));
#733=CARTESIAN_POINT('Ctrl Pts',(-7.17087213616523,190.87379055128,2.21093899485705));
#734=CARTESIAN_POINT('Ctrl Pts',(-7.21281294639898,190.809155844927,2.06440202409992));
#735=CARTESIAN_POINT('Ctrl Pts',(-7.2563597607299,190.74204613624,1.91225383662786));
#736=CARTESIAN_POINT('Ctrl Pts',(-7.29515405471514,190.674628800622,1.75849416561916));
#737=CARTESIAN_POINT('Ctrl Pts',(-7.32904944559233,190.607105531561,1.60357741968119));
#738=CARTESIAN_POINT('Ctrl Pts',(-7.36169037413291,190.542081286575,1.45439411472324));
#739=CARTESIAN_POINT('Ctrl Pts',(-7.38978847549664,190.476959054234,1.30413842461194));
#740=CARTESIAN_POINT('Ctrl Pts',(-7.41326423358634,190.411920847683,1.15323012442364));
#741=CARTESIAN_POINT('Ctrl Pts',(-7.43673590800807,190.346893954693,1.00234807511892));
#742=CARTESIAN_POINT('Ctrl Pts',(-7.45558679680081,190.281951283188,0.850814170351292));
#743=CARTESIAN_POINT('Ctrl Pts',(-7.46978916139915,190.217273190524,0.69905378984192));
#744=CARTESIAN_POINT('Ctrl Pts',(-7.48399533711969,190.15257774187,0.547252685314279));
#745=CARTESIAN_POINT('Ctrl Pts',(-7.493550535944,190.088147231021,0.395225509155809));
#746=CARTESIAN_POINT('Ctrl Pts',(-7.49847882953778,190.024157275818,0.243395891136868));
#747=CARTESIAN_POINT('Ctrl Pts',(-7.49904738356042,190.01677505604,0.225880023131504));
#748=CARTESIAN_POINT('Ctrl Pts',(-7.49955441349822,190.009398692253,0.208366777073135));
#749=CARTESIAN_POINT('Ctrl Pts',(-7.5,190.002028447915,0.190856796705286));
#750=CARTESIAN_POINT('Ctrl Pts',(-7.50386255306115,189.938139708658,0.0390720635508336));
#751=CARTESIAN_POINT('Ctrl Pts',(-7.50312239555638,189.87379055128,-0.113193416375283));
#752=CARTESIAN_POINT('Ctrl Pts',(-7.4977280621597,189.809155844927,-0.265518780412243));
#753=CARTESIAN_POINT('Ctrl Pts',(-7.49212716810079,189.74204613624,-0.423677011229148));
#754=CARTESIAN_POINT('Ctrl Pts',(-7.48150838279932,189.674628800622,-0.581899244411572));
#755=CARTESIAN_POINT('Ctrl Pts',(-7.46587290795734,189.60710553156,-0.739708076931111));
#756=CARTESIAN_POINT('Ctrl Pts',(-7.45081609923473,189.542081286575,-0.891676432865303));
#757=CARTESIAN_POINT('Ctrl Pts',(-7.43110741988625,189.476959054234,-1.04326087688739));
#758=CARTESIAN_POINT('Ctrl Pts',(-7.40680096324194,189.411920847682,-1.19403760735031));
#759=CARTESIAN_POINT('Ctrl Pts',(-7.38249873476802,189.346893954693,-1.3447881098148));
#760=CARTESIAN_POINT('Ctrl Pts',(-7.35360044359543,189.281951283189,-1.49473066237826));
#761=CARTESIAN_POINT('Ctrl Pts',(-7.32021115834367,189.217273190526,-1.64345213319688));
#762=CARTESIAN_POINT('Ctrl Pts',(-7.28681291327052,189.152577741871,-1.79221351256119));
#763=CARTESIAN_POINT('Ctrl Pts',(-7.24892146633721,189.088147231023,-1.93975266792177));
#764=CARTESIAN_POINT('Ctrl Pts',(-7.20669061985663,189.02415727582,-2.08567414197882));
#765=CARTESIAN_POINT('Ctrl Pts',(-7.20181864597947,189.016775056041,-2.10250841524041));
#766=CARTESIAN_POINT('Ctrl Pts',(-7.19688896944668,189.009398692253,-2.11932118289446));
#767=CARTESIAN_POINT('Ctrl Pts',(-7.19190186588755,189.002028447915,-2.13611185762632));
#768=CARTESIAN_POINT('Ctrl Pts',(-7.14867131011472,188.938139708658,-2.28166131170383));
#769=CARTESIAN_POINT('Ctrl Pts',(-7.10091475754315,188.873790551281,-2.42624566734616));
#770=CARTESIAN_POINT('Ctrl Pts',(-7.0487133154537,188.809155844928,-2.56944875671694));
#771=CARTESIAN_POINT('Ctrl Pts',(-6.99451296753918,188.742046136241,-2.71813540129337));
#772=CARTESIAN_POINT('Ctrl Pts',(-6.93552054364173,188.674628800623,-2.8653323020667));
#773=CARTESIAN_POINT('Ctrl Pts',(-6.87188471229685,188.607105531561,-3.01058579312224));
#774=CARTESIAN_POINT('Ctrl Pts',(-6.81060403165581,188.542081286576,-3.15046347852764));
#775=CARTESIAN_POINT('Ctrl Pts',(-6.74501779444825,188.476959054235,-3.28853853492835));
#776=CARTESIAN_POINT('Ctrl Pts',(-6.67530840839942,188.411920847683,-3.42442461876454));
#777=CARTESIAN_POINT('Ctrl Pts',(-6.60561114847652,188.346893954694,-3.560287064869));
#778=CARTESIAN_POINT('Ctrl Pts',(-6.53179244342476,188.281951283189,-3.69396084347412));
#779=CARTESIAN_POINT('Ctrl Pts',(-6.4540798842,188.217273190526,-3.82508551083678));
#780=CARTESIAN_POINT('Ctrl Pts',(-6.37634647125945,188.152577741871,-3.95624536474554));
#781=CARTESIAN_POINT('Ctrl Pts',(-6.29471745739878,188.088147231022,-4.08485433881718));
#782=CARTESIAN_POINT('Ctrl Pts',(-6.20946132033607,188.024157275818,-4.21058385833828));
#783=CARTESIAN_POINT('Ctrl Pts',(-6.19962572130782,188.01677505604,-4.22508868089568));
#784=CARTESIAN_POINT('Ctrl Pts',(-6.18974188939115,188.009398692253,-4.23955521930367));
#785=CARTESIAN_POINT('Ctrl Pts',(-6.17981026821527,188.002028447915,-4.25398300016699));
#786=CARTESIAN_POINT('Ctrl Pts',(-6.09371831161279,187.938139708658,-4.37904978050011));
#787=CARTESIAN_POINT('Ctrl Pts',(-6.00362010807988,187.873790551281,-4.50180008775034));
#788=CARTESIAN_POINT('Ctrl Pts',(-5.90972139815848,187.809155844928,-4.62186318631311));
#789=CARTESIAN_POINT('Ctrl Pts',(-5.81222710407815,187.742046136241,-4.74652375991708));
#790=CARTESIAN_POINT('Ctrl Pts',(-5.71063563106011,187.674628800624,-4.86828667005243));
#791=CARTESIAN_POINT('Ctrl Pts',(-5.60522856176118,187.607105531562,-4.98676639589878));
#792=CARTESIAN_POINT('Ctrl Pts',(-5.50372258919049,187.542081286576,-5.10086120834287));
#793=CARTESIAN_POINT('Ctrl Pts',(-5.39867883198795,187.476959054235,-5.21191112857629));
#794=CARTESIAN_POINT('Ctrl Pts',(-5.29039015693491,187.411920847684,-5.31960508912596));
#795=CARTESIAN_POINT('Ctrl Pts',(-5.18212031897362,187.346893954694,-5.42728031603598));
#796=CARTESIAN_POINT('Ctrl Pts',(-5.07060708921829,187.28195128319,-5.53160039987254));
#797=CARTESIAN_POINT('Ctrl Pts',(-4.9561783027727,187.217273190527,-5.63229286773812));
#798=CARTESIAN_POINT('Ctrl Pts',(-4.84171881002545,187.152577741872,-5.73301235584388));
#799=CARTESIAN_POINT('Ctrl Pts',(-4.72434264585857,187.088147231023,-5.83010200617073));
#800=CARTESIAN_POINT('Ctrl Pts',(-4.60440668292569,187.024157275821,-5.92333228977387));
#801=CARTESIAN_POINT('Ctrl Pts',(-4.59057023570601,187.016775056042,-5.93408782853645));
#802=CARTESIAN_POINT('Ctrl Pts',(-4.57669974673625,187.009398692254,-5.94479205212704));
#803=CARTESIAN_POINT('Ctrl Pts',(-4.56279578422009,187.002028447915,-5.95544464740895));
#804=CARTESIAN_POINT('Ctrl Pts',(-4.44226970733713,186.938139708658,-6.04778634614834));
#805=CARTESIAN_POINT('Ctrl Pts',(-4.31864929275469,186.87379055128,-6.1366869496822));
#806=CARTESIAN_POINT('Ctrl Pts',(-4.19224477495805,186.809155844927,-6.22185744482188));
#807=CARTESIAN_POINT('Ctrl Pts',(-4.0609999554994,186.74204613624,-6.31028930194741));
#808=CARTESIAN_POINT('Ctrl Pts',(-3.9267539145694,186.674628800622,-6.39469921942832));
#809=CARTESIAN_POINT('Ctrl Pts',(-3.78989358567389,186.607105531561,-6.47480755900255));
#810=CARTESIAN_POINT('Ctrl Pts',(-3.65809843300279,186.542081286575,-6.55195110329779));
#811=CARTESIAN_POINT('Ctrl Pts',(-3.52387957064348,186.476959054235,-6.62510554744101));
#812=CARTESIAN_POINT('Ctrl Pts',(-3.38761165659234,186.411920847683,-6.69406554949743));
#813=CARTESIAN_POINT('Ctrl Pts',(-3.25136744669377,186.346893954695,-6.76301355578491));
#814=CARTESIAN_POINT('Ctrl Pts',(-3.11307538412286,186.28195128319,-6.82776836820559));
#815=CARTESIAN_POINT('Ctrl Pts',(-2.97313145734719,186.217273190528,-6.88817215625315));
#816=CARTESIAN_POINT('Ctrl Pts',(-2.83314997742771,186.152577741873,-6.94859215330807));
#817=CARTESIAN_POINT('Ctrl Pts',(-2.69151625970919,186.088147231024,-7.00465866845454));
#818=CARTESIAN_POINT('Ctrl Pts',(-2.54864063859899,186.024157275821,-7.05626368640871));
#819=CARTESIAN_POINT('Ctrl Pts',(-2.53215775104719,186.016775056042,-7.06221711430242));
#820=CARTESIAN_POINT('Ctrl Pts',(-2.51565834512738,186.009398692254,-7.06811121908813));
#821=CARTESIAN_POINT('Ctrl Pts',(-2.49914305799789,186.002028447915,-7.07394587853975));
#822=CARTESIAN_POINT('Ctrl Pts',(-2.35598079299478,185.938139708658,-7.12452344682949));
#823=CARTESIAN_POINT('Ctrl Pts',(-2.21093899485675,185.87379055128,-7.17087213616532));
#824=CARTESIAN_POINT('Ctrl Pts',(-2.06440202409945,185.809155844927,-7.21281294639912));
#825=CARTESIAN_POINT('Ctrl Pts',(-1.91225383662743,185.74204613624,-7.25635976073001));
#826=CARTESIAN_POINT('Ctrl Pts',(-1.75849416561874,185.674628800622,-7.29515405471524));
#827=CARTESIAN_POINT('Ctrl Pts',(-1.60357741968081,185.60710553156,-7.32904944559241));
#828=CARTESIAN_POINT('Ctrl Pts',(-1.45439411472211,185.542081286575,-7.36169037413315));
#829=CARTESIAN_POINT('Ctrl Pts',(-1.30413842461007,185.476959054234,-7.38978847549698));
#830=CARTESIAN_POINT('Ctrl Pts',(-1.15323012442101,185.411920847682,-7.41326423358675));
#831=CARTESIAN_POINT('Ctrl Pts',(-1.002348075116,185.346893954692,-7.43673590800846));
#832=CARTESIAN_POINT('Ctrl Pts',(-0.850814170348105,185.281951283187,-7.45558679680118));
#833=CARTESIAN_POINT('Ctrl Pts',(-0.699053789838449,185.217273190523,-7.46978916139948));
#834=CARTESIAN_POINT('Ctrl Pts',(-0.547252685310788,185.152577741868,-7.48399533711995));
#835=CARTESIAN_POINT('Ctrl Pts',(-0.395225509152289,185.088147231019,-7.49355053594419));
#836=CARTESIAN_POINT('Ctrl Pts',(-0.243395891133334,185.024157275817,-7.4984788295379));
#837=CARTESIAN_POINT('Ctrl Pts',(-0.225880023129145,185.016775056039,-7.49904738356049));
#838=CARTESIAN_POINT('Ctrl Pts',(-0.208366777071962,185.009398692252,-7.49955441349825));
#839=CARTESIAN_POINT('Ctrl Pts',(-0.190856796705286,185.002028447915,-7.5));
#840=CARTESIAN_POINT('Ctrl Pts',(-0.0390720635516772,184.938139708658,-7.50386255306113));
#841=CARTESIAN_POINT('Ctrl Pts',(0.113193416373591,184.873790551281,-7.50312239555639));
#842=CARTESIAN_POINT('Ctrl Pts',(0.265518780409704,184.809155844928,-7.49772806215979));
#843=CARTESIAN_POINT('Ctrl Pts',(0.42367701122682,184.742046136241,-7.49212716810092));
#844=CARTESIAN_POINT('Ctrl Pts',(0.581899244409438,184.674628800623,-7.48150838279949));
#845=CARTESIAN_POINT('Ctrl Pts',(0.739708076929191,184.607105531561,-7.46587290795754));
#846=CARTESIAN_POINT('Ctrl Pts',(0.891676432862843,184.542081286576,-7.45081609923501));
#847=CARTESIAN_POINT('Ctrl Pts',(1.04326087688443,184.476959054235,-7.43110741988665));
#848=CARTESIAN_POINT('Ctrl Pts',(1.19403760734682,184.411920847684,-7.4068009632425));
#849=CARTESIAN_POINT('Ctrl Pts',(1.34478810981303,184.346893954694,-7.38249873476838));
#850=CARTESIAN_POINT('Ctrl Pts',(1.49473066237817,184.281951283189,-7.35360044359548));
#851=CARTESIAN_POINT('Ctrl Pts',(1.64345213319847,184.217273190525,-7.32021115834331));
#852=CARTESIAN_POINT('Ctrl Pts',(1.79221351256205,184.152577741871,-7.28681291327029));
#853=CARTESIAN_POINT('Ctrl Pts',(1.93975266792193,184.088147231022,-7.24892146633715));
#854=CARTESIAN_POINT('Ctrl Pts',(2.08567414197828,184.02415727582,-7.20669061985679));
#855=CARTESIAN_POINT('Ctrl Pts',(2.10250841524006,184.016775056042,-7.20181864597957));
#856=CARTESIAN_POINT('Ctrl Pts',(2.11932118289428,184.009398692253,-7.19688896944673));
#857=CARTESIAN_POINT('Ctrl Pts',(2.13611185762632,184.002028447915,-7.19190186588755));
#858=CARTESIAN_POINT('Ctrl Pts',(2.28166131170458,183.938139708658,-7.14867131011449));
#859=CARTESIAN_POINT('Ctrl Pts',(2.42624566734765,183.87379055128,-7.10091475754266));
#860=CARTESIAN_POINT('Ctrl Pts',(2.56944875671915,183.809155844927,-7.0487133154529));
#861=CARTESIAN_POINT('Ctrl Pts',(2.71813540129538,183.74204613624,-6.9945129675384));
#862=CARTESIAN_POINT('Ctrl Pts',(2.86533230206852,183.674628800622,-6.93552054364098));
#863=CARTESIAN_POINT('Ctrl Pts',(3.01058579312386,183.60710553156,-6.87188471229614));
#864=CARTESIAN_POINT('Ctrl Pts',(3.15046347852959,183.542081286575,-6.81060403165491));
#865=CARTESIAN_POINT('Ctrl Pts',(3.28853853493061,183.476959054234,-6.74501779444716));
#866=CARTESIAN_POINT('Ctrl Pts',(3.4244246187671,183.411920847682,-6.6753084083981));
#867=CARTESIAN_POINT('Ctrl Pts',(3.5602870648721,183.346893954692,-6.60561114847487));
#868=CARTESIAN_POINT('Ctrl Pts',(3.69396084347772,183.281951283188,-6.53179244342274));
#869=CARTESIAN_POINT('Ctrl Pts',(3.82508551084086,183.217273190524,-6.45407988419758));
#870=CARTESIAN_POINT('Ctrl Pts',(3.95624536474775,183.15257774187,-6.37634647125802));
#871=CARTESIAN_POINT('Ctrl Pts',(4.08485433881761,183.088147231021,-6.29471745739845));
#872=CARTESIAN_POINT('Ctrl Pts',(4.21058385833698,183.024157275819,-6.20946132033695));
#873=CARTESIAN_POINT('Ctrl Pts',(4.22508868089482,183.016775056041,-6.19962572130841));
#874=CARTESIAN_POINT('Ctrl Pts',(4.23955521930325,183.009398692253,-6.18974188939143));
#875=CARTESIAN_POINT('Ctrl Pts',(4.25398300016701,183.002028447915,-6.17981026821526));
#876=CARTESIAN_POINT('Ctrl Pts',(4.37904978050103,182.938139708658,-6.09371831161216));
#877=CARTESIAN_POINT('Ctrl Pts',(4.50180008775213,182.87379055128,-6.00362010807857));
#878=CARTESIAN_POINT('Ctrl Pts',(4.62186318631574,182.809155844927,-5.90972139815642));
#879=CARTESIAN_POINT('Ctrl Pts',(4.74652375991945,182.74204613624,-5.81222710407621));
#880=CARTESIAN_POINT('Ctrl Pts',(4.86828667005454,182.674628800622,-5.7106356310583));
#881=CARTESIAN_POINT('Ctrl Pts',(4.98676639590065,182.607105531561,-5.60522856175951));
#882=CARTESIAN_POINT('Ctrl Pts',(5.10086120834469,182.542081286575,-5.5037225891888));
#883=CARTESIAN_POINT('Ctrl Pts',(5.21191112857806,182.476959054234,-5.39867883198624));
#884=CARTESIAN_POINT('Ctrl Pts',(5.31960508912767,182.411920847683,-5.29039015693319));
#885=CARTESIAN_POINT('Ctrl Pts',(5.42728031603767,182.346893954693,-5.18212031897185));
#886=CARTESIAN_POINT('Ctrl Pts',(5.53160039987421,182.281951283189,-5.07060708921647));
#887=CARTESIAN_POINT('Ctrl Pts',(5.63229286773977,182.217273190526,-4.95617830277083));
#888=CARTESIAN_POINT('Ctrl Pts',(5.73301235584584,182.152577741871,-4.84171881002315));
#889=CARTESIAN_POINT('Ctrl Pts',(5.83010200617298,182.088147231022,-4.72434264585582));
#890=CARTESIAN_POINT('Ctrl Pts',(5.92333228977637,182.024157275819,-4.60440668292248));
#891=CARTESIAN_POINT('Ctrl Pts',(5.9340878285381,182.016775056041,-4.59057023570386));
#892=CARTESIAN_POINT('Ctrl Pts',(5.94479205212786,182.009398692253,-4.57669974673518));
#893=CARTESIAN_POINT('Ctrl Pts',(5.95544464740895,182.002028447915,-4.56279578422009));
#894=CARTESIAN_POINT('Ctrl Pts',(6.04778634614845,181.938139708658,-4.442269707337));
#895=CARTESIAN_POINT('Ctrl Pts',(6.1366869496824,181.87379055128,-4.3186492927544));
#896=CARTESIAN_POINT('Ctrl Pts',(6.22185744482218,181.809155844927,-4.19224477495761));
#897=CARTESIAN_POINT('Ctrl Pts',(6.31028930194767,181.74204613624,-4.06099995549899));
#898=CARTESIAN_POINT('Ctrl Pts',(6.39469921942856,181.674628800622,-3.92675391456902));
#899=CARTESIAN_POINT('Ctrl Pts',(6.47480755900275,181.60710553156,-3.78989358567354));
#900=CARTESIAN_POINT('Ctrl Pts',(6.5519511032983,181.542081286575,-3.65809843300192));
#901=CARTESIAN_POINT('Ctrl Pts',(6.62510554744178,181.476959054234,-3.52387957064205));
#902=CARTESIAN_POINT('Ctrl Pts',(6.69406554949843,181.411920847682,-3.38761165659035));
#903=CARTESIAN_POINT('Ctrl Pts',(6.76301355578636,181.346893954693,-3.25136744669082));
#904=CARTESIAN_POINT('Ctrl Pts',(6.8277683682074,181.281951283189,-3.11307538411894));
#905=CARTESIAN_POINT('Ctrl Pts',(6.88817215625527,181.217273190526,-2.97313145734227));
#906=CARTESIAN_POINT('Ctrl Pts',(6.94859215331014,181.152577741871,-2.83314997742263));
#907=CARTESIAN_POINT('Ctrl Pts',(7.00465866845655,181.088147231021,-2.69151625970395));
#908=CARTESIAN_POINT('Ctrl Pts',(7.05626368641066,181.024157275818,-2.54864063859361));
#909=CARTESIAN_POINT('Ctrl Pts',(7.0622171143037,181.01677505604,-2.5321577510436));
#910=CARTESIAN_POINT('Ctrl Pts',(7.06811121908876,181.009398692253,-2.51565834512559));
#911=CARTESIAN_POINT('Ctrl Pts',(7.07394587853975,181.002028447915,-2.4991430579979));
#912=CARTESIAN_POINT('Ctrl Pts',(7.12452344682943,180.938139708658,-2.35598079299495));
#913=CARTESIAN_POINT('Ctrl Pts',(7.17087213616523,180.87379055128,-2.21093899485704));
#914=CARTESIAN_POINT('Ctrl Pts',(7.21281294639899,180.809155844927,-2.0644020240999));
#915=CARTESIAN_POINT('Ctrl Pts',(7.2563597607299,180.74204613624,-1.91225383662784));
#916=CARTESIAN_POINT('Ctrl Pts',(7.29515405471515,180.674628800622,-1.75849416561912));
#917=CARTESIAN_POINT('Ctrl Pts',(7.32904944559233,180.607105531561,-1.60357741968115));
#918=CARTESIAN_POINT('Ctrl Pts',(7.36169037413299,180.542081286575,-1.45439411472287));
#919=CARTESIAN_POINT('Ctrl Pts',(7.38978847549676,180.476959054234,-1.30413842461125));
#920=CARTESIAN_POINT('Ctrl Pts',(7.4132642335865,180.411920847682,-1.15323012442261));
#921=CARTESIAN_POINT('Ctrl Pts',(7.43673590800803,180.346893954693,-1.00234807511903));
#922=CARTESIAN_POINT('Ctrl Pts',(7.45558679680064,180.281951283189,-0.850814170352573));
#923=CARTESIAN_POINT('Ctrl Pts',(7.46978916139892,180.217273190526,-0.699053789844363));
#924=CARTESIAN_POINT('Ctrl Pts',(7.48399533711951,180.152577741871,-0.547252685316772));
#925=CARTESIAN_POINT('Ctrl Pts',(7.49355053594387,180.088147231022,-0.39522550915836));
#926=CARTESIAN_POINT('Ctrl Pts',(7.4984788295377,180.024157275819,-0.243395891139465));
#927=CARTESIAN_POINT('Ctrl Pts',(7.49904738356037,180.016775056041,-0.225880023133238));
#928=CARTESIAN_POINT('Ctrl Pts',(7.49955441349819,180.009398692253,-0.208366777073998));
#929=CARTESIAN_POINT('Ctrl Pts',(7.5,180.002028447915,-0.190856796705287));
#930=CARTESIAN_POINT('Ctrl Pts',(7.50386255306115,179.938139708658,-0.0390720635508177));
#931=CARTESIAN_POINT('Ctrl Pts',(7.50312239555638,179.87379055128,0.113193416375312));
#932=CARTESIAN_POINT('Ctrl Pts',(7.49772806215969,179.809155844927,0.265518780412289));
#933=CARTESIAN_POINT('Ctrl Pts',(7.49212716810078,179.74204613624,0.42367701122919));
#934=CARTESIAN_POINT('Ctrl Pts',(7.48150838279932,179.674628800622,0.581899244411606));
#935=CARTESIAN_POINT('Ctrl Pts',(7.46587290795734,179.60710553156,0.739708076931141));
#936=CARTESIAN_POINT('Ctrl Pts',(7.45081609923473,179.542081286575,0.891676432865285));
#937=CARTESIAN_POINT('Ctrl Pts',(7.43110741988625,179.476959054234,1.04326087688732));
#938=CARTESIAN_POINT('Ctrl Pts',(7.40680096324196,179.411920847682,1.1940376073502));
#939=CARTESIAN_POINT('Ctrl Pts',(7.38249873476815,179.346893954694,1.34478810981401));
#940=CARTESIAN_POINT('Ctrl Pts',(7.35360044359571,179.281951283189,1.4947306623768));
#941=CARTESIAN_POINT('Ctrl Pts',(7.32021115834415,179.217273190527,1.64345213319477));
#942=CARTESIAN_POINT('Ctrl Pts',(7.28681291327109,179.152577741872,1.79221351255885));
#943=CARTESIAN_POINT('Ctrl Pts',(7.24892146633789,179.088147231024,1.93975266791923));
#944=CARTESIAN_POINT('Ctrl Pts',(7.20669061985743,179.024157275821,2.08567414197607));
#945=CARTESIAN_POINT('Ctrl Pts',(7.20181864598001,179.016775056042,2.10250841523858));
#946=CARTESIAN_POINT('Ctrl Pts',(7.19688896944695,179.009398692254,2.11932118289354));
#947=CARTESIAN_POINT('Ctrl Pts',(7.19190186588755,179.002028447915,2.13611185762632));
#948=CARTESIAN_POINT('Ctrl Pts',(7.14867131011455,178.938139708658,2.2816613117044));
#949=CARTESIAN_POINT('Ctrl Pts',(7.10091475754278,178.87379055128,2.42624566734728));
#950=CARTESIAN_POINT('Ctrl Pts',(7.0487133154531,178.809155844927,2.56944875671861));
#951=CARTESIAN_POINT('Ctrl Pts',(6.99451296753859,178.74204613624,2.71813540129489));
#952=CARTESIAN_POINT('Ctrl Pts',(6.93552054364116,178.674628800623,2.86533230206808));
#953=CARTESIAN_POINT('Ctrl Pts',(6.87188471229631,178.607105531561,3.01058579312346));
#954=CARTESIAN_POINT('Ctrl Pts',(6.81060403165535,178.542081286575,3.15046347852861));
#955=CARTESIAN_POINT('Ctrl Pts',(6.7450177944479,178.476959054234,3.28853853492906));
#956=CARTESIAN_POINT('Ctrl Pts',(6.67530840839917,178.411920847683,3.42442461876501));
#957=CARTESIAN_POINT('Ctrl Pts',(6.60561114847623,178.346893954694,3.56028706486955));
#958=CARTESIAN_POINT('Ctrl Pts',(6.53179244342441,178.281951283189,3.69396084347474));
#959=CARTESIAN_POINT('Ctrl Pts',(6.4540798841996,178.217273190526,3.82508551083747));
#960=CARTESIAN_POINT('Ctrl Pts',(6.37634647126001,178.152577741872,3.95624536474455));
#961=CARTESIAN_POINT('Ctrl Pts',(6.29471745740041,178.088147231023,4.08485433881459));
#962=CARTESIAN_POINT('Ctrl Pts',(6.20946132033887,178.02415727582,4.21058385833414));
#963=CARTESIAN_POINT('Ctrl Pts',(6.1996257213097,178.016775056042,4.22508868089293));
#964=CARTESIAN_POINT('Ctrl Pts',(6.18974188939208,178.009398692254,4.23955521930231));
#965=CARTESIAN_POINT('Ctrl Pts',(6.17981026821526,178.002028447915,4.25398300016701));
#966=CARTESIAN_POINT('Ctrl Pts',(6.09371831161207,177.938139708658,4.37904978050116));
#967=CARTESIAN_POINT('Ctrl Pts',(6.0036201080784,177.87379055128,4.50180008775236));
#968=CARTESIAN_POINT('Ctrl Pts',(5.90972139815616,177.809155844927,4.62186318631608));
#969=CARTESIAN_POINT('Ctrl Pts',(5.81222710407596,177.74204613624,4.74652375991976));
#970=CARTESIAN_POINT('Ctrl Pts',(5.71063563105806,177.674628800622,4.86828667005482));
#971=CARTESIAN_POINT('Ctrl Pts',(5.6052285617593,177.60710553156,4.98676639590089));
#972=CARTESIAN_POINT('Ctrl Pts',(5.5037225891889,177.542081286575,5.10086120834457));
#973=CARTESIAN_POINT('Ctrl Pts',(5.39867883198667,177.476959054235,5.2119111285776));
#974=CARTESIAN_POINT('Ctrl Pts',(5.29039015693398,177.411920847683,5.31960508912689));
#975=CARTESIAN_POINT('Ctrl Pts',(5.18212031897253,177.346893954694,5.42728031603702));
#976=CARTESIAN_POINT('Ctrl Pts',(5.07060708921705,177.281951283189,5.53160039987369));
#977=CARTESIAN_POINT('Ctrl Pts',(4.95617830277129,177.217273190526,5.63229286773936));
#978=CARTESIAN_POINT('Ctrl Pts',(4.84171881002452,177.152577741872,5.73301235584465));
#979=CARTESIAN_POINT('Ctrl Pts',(4.72434264585812,177.088147231023,5.83010200617108));
#980=CARTESIAN_POINT('Ctrl Pts',(4.60440668292578,177.024157275821,5.92333228977381));
#981=CARTESIAN_POINT('Ctrl Pts',(4.59057023570606,177.016775056042,5.93408782853641));
#982=CARTESIAN_POINT('Ctrl Pts',(4.57669974673629,177.009398692254,5.94479205212701));
#983=CARTESIAN_POINT('Ctrl Pts',(4.56279578422009,177.002028447915,5.95544464740895));
#984=CARTESIAN_POINT('Ctrl Pts',(4.44226970733713,176.938139708658,6.04778634614834));
#985=CARTESIAN_POINT('Ctrl Pts',(4.31864929275468,176.87379055128,6.1366869496822));
#986=CARTESIAN_POINT('Ctrl Pts',(4.19224477495804,176.809155844927,6.22185744482189));
#987=CARTESIAN_POINT('Ctrl Pts',(4.06099995549939,176.74204613624,6.31028930194742));
#988=CARTESIAN_POINT('Ctrl Pts',(3.92675391456939,176.674628800622,6.39469921942833));
#989=CARTESIAN_POINT('Ctrl Pts',(3.78989358567388,176.607105531561,6.47480755900255));
#990=CARTESIAN_POINT('Ctrl Pts',(3.65809843300261,176.542081286575,6.5519511032979));
#991=CARTESIAN_POINT('Ctrl Pts',(3.52387957064311,176.476959054234,6.62510554744121));
#992=CARTESIAN_POINT('Ctrl Pts',(3.38761165659179,176.411920847683,6.69406554949771));
#993=CARTESIAN_POINT('Ctrl Pts',(3.25136744669221,176.346893954694,6.76301355578569));
#994=CARTESIAN_POINT('Ctrl Pts',(3.11307538412028,176.281951283189,6.82776836820679));
#995=CARTESIAN_POINT('Ctrl Pts',(2.97313145734355,176.217273190526,6.88817215625472));
#996=CARTESIAN_POINT('Ctrl Pts',(2.83314997742486,176.152577741872,6.94859215330921));
#997=CARTESIAN_POINT('Ctrl Pts',(2.69151625970714,176.088147231023,7.00465866845531));
#998=CARTESIAN_POINT('Ctrl Pts',(2.54864063859777,176.02415727582,7.05626368640916));
#999=CARTESIAN_POINT('Ctrl Pts',(2.53215775104638,176.016775056042,7.06221711430271));
#1000=CARTESIAN_POINT('Ctrl Pts',(2.51565834512697,176.009398692253,7.06811121908827));
#1001=CARTESIAN_POINT('Ctrl Pts',(2.49914305799789,176.002028447915,7.07394587853975));
#1002=CARTESIAN_POINT('Ctrl Pts',(2.35598079328146,175.938139708785,7.12452344672821));
#1003=CARTESIAN_POINT('Ctrl Pts',(2.21093899543762,175.873790551538,7.17087213597972));
#1004=CARTESIAN_POINT('Ctrl Pts',(2.06440202497974,175.809155845315,7.21281294614716));
#1005=CARTESIAN_POINT('Ctrl Pts',(1.91225491695072,175.742046612748,7.25635945154735));
#1006=CARTESIAN_POINT('Ctrl Pts',(1.75849634827299,175.674629757621,7.2951535041046));
#1007=CARTESIAN_POINT('Ctrl Pts',(1.60358071781314,175.607106969111,7.32904872396865));
#1008=CARTESIAN_POINT('Ctrl Pts',(1.4543974295954,175.542082725982,7.36168971919407));
#1009=CARTESIAN_POINT('Ctrl Pts',(1.30414175318146,175.476960494159,7.38978788807506));
#1010=CARTESIAN_POINT('Ctrl Pts',(1.15323346356763,175.411922286781,7.41326371413808));
#1011=CARTESIAN_POINT('Ctrl Pts',(1.0023514247394,175.346895392924,7.43673545653627));
#1012=CARTESIAN_POINT('Ctrl Pts',(0.850817527325577,175.281952719209,7.45558641375475));
#1013=CARTESIAN_POINT('Ctrl Pts',(0.699057151026253,175.217274623013,7.46978884684485));
#1014=CARTESIAN_POINT('Ctrl Pts',(0.547256052215635,175.152579171467,7.4839950909346));
#1015=CARTESIAN_POINT('Ctrl Pts',(0.395228878633319,175.088148656398,7.49355035828583));
#1016=CARTESIAN_POINT('Ctrl Pts',(0.243399260074249,175.024158695687,7.49847872018344));
#1017=CARTESIAN_POINT('Ctrl Pts',(0.225886742935279,175.016777887553,7.49904717331543));
#1018=CARTESIAN_POINT('Ctrl Pts',(0.208376846698734,175.009402933151,7.49955412589778));
#1019=CARTESIAN_POINT('Ctrl Pts',(0.190870214739035,175.002034095791,7.4999996585316));
#1020=CARTESIAN_POINT('',(0.000256710970817156,177.995967593475,7.49999999788466));
#1021=CARTESIAN_POINT('Origin',(-5.20512090547431E-6,178.000081808606,-1851.55088195117));
#1022=CARTESIAN_POINT('',(-1.89809114034451E-16,197.99585953923,7.50000000439337));
#1023=CARTESIAN_POINT('Ctrl Pts',(5.38866871829646E-16,197.99585953923,
7.50000000439337));
#1024=CARTESIAN_POINT('Ctrl Pts',(-1.18775172812192,197.495912211348,7.50000000439337));
#1025=CARTESIAN_POINT('Ctrl Pts',(-2.317383311169,196.995967593475,7.13300320026677));
#1026=CARTESIAN_POINT('Ctrl Pts',(-3.44714003087638,196.495967593475,6.76596574150984));
#1027=CARTESIAN_POINT('Ctrl Pts',(-4.40818170865423,195.995967593475,6.06777834873578));
#1028=CARTESIAN_POINT('Ctrl Pts',(-5.36922338643209,195.495967593475,5.36959095596173));
#1029=CARTESIAN_POINT('Ctrl Pts',(-6.06747656688843,194.995967593475,4.40859707573286));
#1030=CARTESIAN_POINT('Ctrl Pts',(-6.76572974734476,194.495967593475,3.447603195504));
#1031=CARTESIAN_POINT('Ctrl Pts',(-7.13284454416054,193.995967593475,2.31787160445521));
#1032=CARTESIAN_POINT('Ctrl Pts',(-7.49995934097631,193.495967593475,1.18814001340642));
#1033=CARTESIAN_POINT('Ctrl Pts',(-7.5,192.995967593475,0.000256710972401669));
#1034=CARTESIAN_POINT('Ctrl Pts',(-7.50004065902369,192.495967593475,-1.18762659146162));
#1035=CARTESIAN_POINT('Ctrl Pts',(-7.13300320026677,191.995967593475,-2.317383311169));
#1036=CARTESIAN_POINT('Ctrl Pts',(-6.76596574150984,191.495967593475,-3.44714003087638));
#1037=CARTESIAN_POINT('Ctrl Pts',(-6.06777834873578,190.995967593475,-4.40818170865423));
#1038=CARTESIAN_POINT('Ctrl Pts',(-5.36959095596173,190.495967593475,-5.36922338643209));
#1039=CARTESIAN_POINT('Ctrl Pts',(-4.40859707573286,189.995967593475,-6.06747656688843));
#1040=CARTESIAN_POINT('Ctrl Pts',(-3.447603195504,189.495967593475,-6.76572974734476));
#1041=CARTESIAN_POINT('Ctrl Pts',(-2.31787160445521,188.995967593475,-7.13284454416054));
#1042=CARTESIAN_POINT('Ctrl Pts',(-1.18814001340642,188.495967593475,-7.49995934097631));
#1043=CARTESIAN_POINT('Ctrl Pts',(-0.000256710972402128,187.995967593475,
-7.5));
#1044=CARTESIAN_POINT('Ctrl Pts',(1.18762659146162,187.495967593475,-7.50004065902369));
#1045=CARTESIAN_POINT('Ctrl Pts',(2.317383311169,186.995967593475,-7.13300320026677));
#1046=CARTESIAN_POINT('Ctrl Pts',(3.44714003087638,186.495967593475,-6.76596574150984));
#1047=CARTESIAN_POINT('Ctrl Pts',(4.40818170865423,185.995967593475,-6.06777834873578));
#1048=CARTESIAN_POINT('Ctrl Pts',(5.36922338643209,185.495967593475,-5.36959095596173));
#1049=CARTESIAN_POINT('Ctrl Pts',(6.06747656688843,184.995967593475,-4.40859707573286));
#1050=CARTESIAN_POINT('Ctrl Pts',(6.76572974734476,184.495967593475,-3.447603195504));
#1051=CARTESIAN_POINT('Ctrl Pts',(7.13284454416054,183.995967593475,-2.31787160445521));
#1052=CARTESIAN_POINT('Ctrl Pts',(7.49995934097631,183.495967593475,-1.18814001340642));
#1053=CARTESIAN_POINT('Ctrl Pts',(7.5,182.995967593475,-0.000256710972402588));
#1054=CARTESIAN_POINT('Ctrl Pts',(7.50004065902369,182.495967593475,1.18762659146162));
#1055=CARTESIAN_POINT('Ctrl Pts',(7.13300320026677,181.995967593475,2.317383311169));
#1056=CARTESIAN_POINT('Ctrl Pts',(6.76596574150984,181.495967593475,3.44714003087638));
#1057=CARTESIAN_POINT('Ctrl Pts',(6.06777834873579,180.995967593475,4.40818170865423));
#1058=CARTESIAN_POINT('Ctrl Pts',(5.36959095596173,180.495967593475,5.36922338643209));
#1059=CARTESIAN_POINT('Ctrl Pts',(4.40859707573286,179.995967593475,6.06747656688843));
#1060=CARTESIAN_POINT('Ctrl Pts',(3.447603195504,179.495967593475,6.76572974734476));
#1061=CARTESIAN_POINT('Ctrl Pts',(2.31787160445521,178.995967593475,7.13284454416054));
#1062=CARTESIAN_POINT('Ctrl Pts',(1.18814001340643,178.495967593475,7.49995934097631));
#1063=CARTESIAN_POINT('Ctrl Pts',(0.00025671097240121,177.995967593475,
7.5));
#1064=CARTESIAN_POINT('',(-4.06843942354914E-7,214.921557632927,7.50242802810186));
#1065=CARTESIAN_POINT('',(-9.18485099360515E-16,240.,7.5));
#1066=CARTESIAN_POINT('Ctrl Pts',(-4.068439266928E-7,214.921557632927,7.50242802810187));
#1067=CARTESIAN_POINT('Ctrl Pts',(-0.152090385416069,214.857323985265,7.50242801985428));
#1068=CARTESIAN_POINT('Ctrl Pts',(-0.304485788638696,214.792702491972,7.49779895914527));
#1069=CARTESIAN_POINT('Ctrl Pts',(-0.456762644215681,214.72787053402,7.48851081348606));
#1070=CARTESIAN_POINT('Ctrl Pts',(-0.609070650331504,214.663025313709,7.47922076779588));
#1071=CARTESIAN_POINT('Ctrl Pts',(-0.761259533138804,214.597969762788,7.46526968655064));
#1072=CARTESIAN_POINT('Ctrl Pts',(-0.91290272043933,214.532885263597,7.44667945730599));
#1073=CARTESIAN_POINT('Ctrl Pts',(-1.0645049306871,214.467818351553,7.42809425151685));
#1074=CARTESIAN_POINT('Ctrl Pts',(-1.21556121279854,214.402722732839,7.40487246128572));
#1075=CARTESIAN_POINT('Ctrl Pts',(-1.36565093134601,214.3377801784,7.37708776215671));
#1076=CARTESIAN_POINT('Ctrl Pts',(-1.51579830432504,214.272812677376,7.3492923900046));
#1077=CARTESIAN_POINT('Ctrl Pts',(-1.66497786162516,214.207998581557,7.31693074896066));
#1078=CARTESIAN_POINT('Ctrl Pts',(-1.8127818777126,214.143517028959,7.28012693438002));
#1079=CARTESIAN_POINT('Ctrl Pts',(-1.92135204017723,214.096151789321,7.25309251248735));
#1080=CARTESIAN_POINT('Ctrl Pts',(-2.02918025203189,214.04896593395,7.22366229239569));
#1081=CARTESIAN_POINT('Ctrl Pts',(-2.13611185762632,214.002028447915,7.19190186588755));
#1082=CARTESIAN_POINT('Ctrl Pts',(-2.28166131170438,213.938139708658,7.14867131011455));
#1083=CARTESIAN_POINT('Ctrl Pts',(-2.42624566734726,213.87379055128,7.10091475754279));
#1084=CARTESIAN_POINT('Ctrl Pts',(-2.56944875671857,213.809155844927,7.04871331545311));
#1085=CARTESIAN_POINT('Ctrl Pts',(-2.71813540129485,213.74204613624,6.99451296753861));
#1086=CARTESIAN_POINT('Ctrl Pts',(-2.86533230206802,213.674628800623,6.93552054364118));
#1087=CARTESIAN_POINT('Ctrl Pts',(-3.01058579312341,213.607105531561,6.87188471229634));
#1088=CARTESIAN_POINT('Ctrl Pts',(-3.15046347852853,213.542081286575,6.81060403165539));
#1089=CARTESIAN_POINT('Ctrl Pts',(-3.28853853492897,213.476959054234,6.74501779444794));
#1090=CARTESIAN_POINT('Ctrl Pts',(-3.4244246187649,213.411920847683,6.67530840839923));
#1091=CARTESIAN_POINT('Ctrl Pts',(-3.56028706486959,213.346893954694,6.60561114847621));
#1092=CARTESIAN_POINT('Ctrl Pts',(-3.69396084347493,213.281951283189,6.53179244342431));
#1093=CARTESIAN_POINT('Ctrl Pts',(-3.8250855108378,213.217273190526,6.4540798841994));
#1094=CARTESIAN_POINT('Ctrl Pts',(-3.95624536474509,213.152577741871,6.37634647125968));
#1095=CARTESIAN_POINT('Ctrl Pts',(-4.08485433881534,213.088147231023,6.29471745739993));
#1096=CARTESIAN_POINT('Ctrl Pts',(-4.21058385833508,213.02415727582,6.20946132033823));
#1097=CARTESIAN_POINT('Ctrl Pts',(-4.22508868089356,213.016775056042,6.19962572130926));
#1098=CARTESIAN_POINT('Ctrl Pts',(-4.23955521930262,213.009398692253,6.18974188939186));
#1099=CARTESIAN_POINT('Ctrl Pts',(-4.25398300016701,213.002028447915,6.17981026821525));
#1100=CARTESIAN_POINT('Ctrl Pts',(-4.37904978050102,212.938139708658,6.09371831161217));
#1101=CARTESIAN_POINT('Ctrl Pts',(-4.50180008775209,212.87379055128,6.00362010807859));
#1102=CARTESIAN_POINT('Ctrl Pts',(-4.62186318631568,212.809155844927,5.90972139815647));
#1103=CARTESIAN_POINT('Ctrl Pts',(-4.74652375991939,212.74204613624,5.81222710407626));
#1104=CARTESIAN_POINT('Ctrl Pts',(-4.86828667005449,212.674628800623,5.71063563105834));
#1105=CARTESIAN_POINT('Ctrl Pts',(-4.9867663959006,212.607105531561,5.60522856175955));
#1106=CARTESIAN_POINT('Ctrl Pts',(-5.10086120834463,212.542081286575,5.50372258918886));
#1107=CARTESIAN_POINT('Ctrl Pts',(-5.21191112857799,212.476959054234,5.39867883198632));
#1108=CARTESIAN_POINT('Ctrl Pts',(-5.31960508912758,212.411920847683,5.29039015693328));
#1109=CARTESIAN_POINT('Ctrl Pts',(-5.42728031603771,212.346893954693,5.18212031897182));
#1110=CARTESIAN_POINT('Ctrl Pts',(-5.53160039987437,212.281951283189,5.07060708921631));
#1111=CARTESIAN_POINT('Ctrl Pts',(-5.63229286774003,212.217273190525,4.95617830277053));
#1112=CARTESIAN_POINT('Ctrl Pts',(-5.73301235584579,212.152577741871,4.84171881002319));
#1113=CARTESIAN_POINT('Ctrl Pts',(-5.83010200617264,212.088147231022,4.72434264585622));
#1114=CARTESIAN_POINT('Ctrl Pts',(-5.92333228977576,212.02415727582,4.60440668292327));
#1115=CARTESIAN_POINT('Ctrl Pts',(-5.9340878285377,212.016775056041,4.59057023570439));
#1116=CARTESIAN_POINT('Ctrl Pts',(-5.94479205212766,212.009398692253,4.57669974673545));
#1117=CARTESIAN_POINT('Ctrl Pts',(-5.95544464740895,212.002028447915,4.5627957842201));
#1118=CARTESIAN_POINT('Ctrl Pts',(-6.04778634614838,211.938139708658,4.44226970733709));
#1119=CARTESIAN_POINT('Ctrl Pts',(-6.13668694968226,211.87379055128,4.3186492927546));
#1120=CARTESIAN_POINT('Ctrl Pts',(-6.22185744482198,211.809155844927,4.19224477495791));
#1121=CARTESIAN_POINT('Ctrl Pts',(-6.3102893019475,211.74204613624,4.06099995549926));
#1122=CARTESIAN_POINT('Ctrl Pts',(-6.39469921942841,211.674628800622,3.92675391456926));
#1123=CARTESIAN_POINT('Ctrl Pts',(-6.47480755900262,211.607105531561,3.78989358567376));
#1124=CARTESIAN_POINT('Ctrl Pts',(-6.55195110329808,211.542081286575,3.65809843300229));
#1125=CARTESIAN_POINT('Ctrl Pts',(-6.62510554744149,211.476959054234,3.52387957064258));
#1126=CARTESIAN_POINT('Ctrl Pts',(-6.69406554949808,211.411920847683,3.38761165659104));
#1127=CARTESIAN_POINT('Ctrl Pts',(-6.76301355578619,211.346893954693,3.25136744669118));
#1128=CARTESIAN_POINT('Ctrl Pts',(-6.8277683682074,211.281951283189,3.11307538411895));
#1129=CARTESIAN_POINT('Ctrl Pts',(-6.88817215625542,211.217273190525,2.97313145734192));
#1130=CARTESIAN_POINT('Ctrl Pts',(-6.94859215330986,211.152577741871,2.83314997742328));
#1131=CARTESIAN_POINT('Ctrl Pts',(-7.00465866845589,211.088147231022,2.69151625970561));
#1132=CARTESIAN_POINT('Ctrl Pts',(-7.05626368640969,211.02415727582,2.5486406385963));
#1133=CARTESIAN_POINT('Ctrl Pts',(-7.06221711430306,211.016775056041,2.53215775104539));
#1134=CARTESIAN_POINT('Ctrl Pts',(-7.06811121908845,211.009398692253,2.51565834512648));
#1135=CARTESIAN_POINT('Ctrl Pts',(-7.07394587853975,211.002028447915,2.49914305799789));
#1136=CARTESIAN_POINT('Ctrl Pts',(-7.12452344682943,210.938139708658,2.35598079299496));
#1137=CARTESIAN_POINT('Ctrl Pts',(-7.17087213616521,210.87379055128,2.2109389948571));
#1138=CARTESIAN_POINT('Ctrl Pts',(-7.21281294639896,210.809155844927,2.06440202409999));
#1139=CARTESIAN_POINT('Ctrl Pts',(-7.25635976072988,210.74204613624,1.91225383662793));
#1140=CARTESIAN_POINT('Ctrl Pts',(-7.29515405471512,210.674628800622,1.75849416561922));
#1141=CARTESIAN_POINT('Ctrl Pts',(-7.32904944559231,210.607105531561,1.60357741968125));
#1142=CARTESIAN_POINT('Ctrl Pts',(-7.3616903741329,210.542081286575,1.4543941147233));
#1143=CARTESIAN_POINT('Ctrl Pts',(-7.38978847549662,210.476959054234,1.30413842461201));
#1144=CARTESIAN_POINT('Ctrl Pts',(-7.41326423358633,210.411920847683,1.15323012442371));
#1145=CARTESIAN_POINT('Ctrl Pts',(-7.43673590800795,210.346893954693,1.00234807511964));
#1146=CARTESIAN_POINT('Ctrl Pts',(-7.45558679680064,210.281951283189,0.85081417035268));
#1147=CARTESIAN_POINT('Ctrl Pts',(-7.46978916139896,210.217273190525,0.699053789843961));
#1148=CARTESIAN_POINT('Ctrl Pts',(-7.48399533711949,210.152577741871,0.54725268531685));
#1149=CARTESIAN_POINT('Ctrl Pts',(-7.49355053594383,210.088147231022,0.395225509158903));
#1150=CARTESIAN_POINT('Ctrl Pts',(-7.49847882953766,210.02415727582,0.243395891140488));
#1151=CARTESIAN_POINT('Ctrl Pts',(-7.49904738356035,210.016775056041,0.225880023133914));
#1152=CARTESIAN_POINT('Ctrl Pts',(-7.49955441349819,210.009398692253,0.208366777074336));
#1153=CARTESIAN_POINT('Ctrl Pts',(-7.5,210.002028447915,0.190856796705278));
#1154=CARTESIAN_POINT('Ctrl Pts',(-7.50386255306115,209.938139708658,0.0390720635509829));
#1155=CARTESIAN_POINT('Ctrl Pts',(-7.50312239555638,209.87379055128,-0.11319341637498));
#1156=CARTESIAN_POINT('Ctrl Pts',(-7.49772806215971,209.809155844927,-0.265518780411782));
#1157=CARTESIAN_POINT('Ctrl Pts',(-7.49212716810081,209.74204613624,-0.423677011228724));
#1158=CARTESIAN_POINT('Ctrl Pts',(-7.48150838279936,209.674628800622,-0.581899244411169));
#1159=CARTESIAN_POINT('Ctrl Pts',(-7.46587290795738,209.607105531561,-0.739708076930746));
#1160=CARTESIAN_POINT('Ctrl Pts',(-7.4508160992348,209.542081286575,-0.891676432864672));
#1161=CARTESIAN_POINT('Ctrl Pts',(-7.43110741988636,209.476959054234,-1.04326087688651));
#1162=CARTESIAN_POINT('Ctrl Pts',(-7.40680096324212,209.411920847683,-1.19403760734917));
#1163=CARTESIAN_POINT('Ctrl Pts',(-7.38249873476809,209.346893954693,-1.34478810981454));
#1164=CARTESIAN_POINT('Ctrl Pts',(-7.35360044359533,209.281951283189,-1.49473066237887));
#1165=CARTESIAN_POINT('Ctrl Pts',(-7.32021115834334,209.217273190525,-1.64345213319835));
#1166=CARTESIAN_POINT('Ctrl Pts',(-7.28681291327022,209.152577741871,-1.79221351256238));
#1167=CARTESIAN_POINT('Ctrl Pts',(-7.24892146633696,209.088147231022,-1.93975266792269));
#1168=CARTESIAN_POINT('Ctrl Pts',(-7.20669061985644,209.02415727582,-2.08567414197946));
#1169=CARTESIAN_POINT('Ctrl Pts',(-7.20181864597934,209.016775056041,-2.10250841524085));
#1170=CARTESIAN_POINT('Ctrl Pts',(-7.19688896944662,209.009398692253,-2.11932118289467));
#1171=CARTESIAN_POINT('Ctrl Pts',(-7.19190186588755,209.002028447915,-2.13611185762632));
#1172=CARTESIAN_POINT('Ctrl Pts',(-7.14867131011455,208.938139708658,-2.28166131170439));
#1173=CARTESIAN_POINT('Ctrl Pts',(-7.10091475754278,208.87379055128,-2.42624566734729));
#1174=CARTESIAN_POINT('Ctrl Pts',(-7.0487133154531,208.809155844927,-2.56944875671861));
#1175=CARTESIAN_POINT('Ctrl Pts',(-6.99451296753859,208.74204613624,-2.71813540129489));
#1176=CARTESIAN_POINT('Ctrl Pts',(-6.93552054364117,208.674628800623,-2.86533230206806));
#1177=CARTESIAN_POINT('Ctrl Pts',(-6.87188471229632,208.607105531561,-3.01058579312345));
#1178=CARTESIAN_POINT('Ctrl Pts',(-6.8106040316553,208.542081286575,-3.15046347852873));
#1179=CARTESIAN_POINT('Ctrl Pts',(-6.74501779444778,208.476959054234,-3.28853853492931));
#1180=CARTESIAN_POINT('Ctrl Pts',(-6.67530840839898,208.411920847683,-3.42442461876539));
#1181=CARTESIAN_POINT('Ctrl Pts',(-6.60561114847592,208.346893954693,-3.56028706487013));
#1182=CARTESIAN_POINT('Ctrl Pts',(-6.53179244342397,208.281951283189,-3.69396084347553));
#1183=CARTESIAN_POINT('Ctrl Pts',(-6.45407988419901,208.217273190525,-3.82508551083845));
#1184=CARTESIAN_POINT('Ctrl Pts',(-6.37634647125933,208.152577741871,-3.95624536474565));
#1185=CARTESIAN_POINT('Ctrl Pts',(-6.29471745739962,208.088147231022,-4.08485433881581));
#1186=CARTESIAN_POINT('Ctrl Pts',(-6.20946132033797,208.02415727582,-4.21058385833547));
#1187=CARTESIAN_POINT('Ctrl Pts',(-6.19962572130909,208.016775056041,-4.22508868089382));
#1188=CARTESIAN_POINT('Ctrl Pts',(-6.18974188939178,208.009398692253,-4.23955521930275));
#1189=CARTESIAN_POINT('Ctrl Pts',(-6.17981026821526,208.002028447915,-4.253983000167));
#1190=CARTESIAN_POINT('Ctrl Pts',(-6.09371831161218,207.938139708658,-4.379049780501));
#1191=CARTESIAN_POINT('Ctrl Pts',(-6.00362010807862,207.87379055128,-4.50180008775205));
#1192=CARTESIAN_POINT('Ctrl Pts',(-5.90972139815651,207.809155844927,-4.62186318631563));
#1193=CARTESIAN_POINT('Ctrl Pts',(-5.81222710407629,207.74204613624,-4.74652375991935));
#1194=CARTESIAN_POINT('Ctrl Pts',(-5.71063563105837,207.674628800623,-4.86828667005446));
#1195=CARTESIAN_POINT('Ctrl Pts',(-5.60522856175958,207.607105531561,-4.98676639590057));
#1196=CARTESIAN_POINT('Ctrl Pts',(-5.50372258918887,207.542081286575,-5.10086120834461));
#1197=CARTESIAN_POINT('Ctrl Pts',(-5.39867883198632,207.476959054234,-5.21191112857799));
#1198=CARTESIAN_POINT('Ctrl Pts',(-5.29039015693326,207.411920847683,-5.3196050891276));
#1199=CARTESIAN_POINT('Ctrl Pts',(-5.18212031897177,207.346893954693,-5.42728031603775));
#1200=CARTESIAN_POINT('Ctrl Pts',(-5.07060708921622,207.281951283189,-5.53160039987444));
#1201=CARTESIAN_POINT('Ctrl Pts',(-4.95617830277041,207.217273190525,-5.63229286774013));
#1202=CARTESIAN_POINT('Ctrl Pts',(-4.8417188100227,207.152577741871,-5.73301235584621));
#1203=CARTESIAN_POINT('Ctrl Pts',(-4.72434264585535,207.088147231022,-5.83010200617336));
#1204=CARTESIAN_POINT('Ctrl Pts',(-4.60440668292199,207.024157275819,-5.92333228977675));
#1205=CARTESIAN_POINT('Ctrl Pts',(-4.59057023570353,207.016775056041,-5.93408782853836));
#1206=CARTESIAN_POINT('Ctrl Pts',(-4.57669974673502,207.009398692253,-5.94479205212799));
#1207=CARTESIAN_POINT('Ctrl Pts',(-4.56279578422009,207.002028447915,-5.95544464740895));
#1208=CARTESIAN_POINT('Ctrl Pts',(-4.44226970733713,206.938139708658,-6.04778634614835));
#1209=CARTESIAN_POINT('Ctrl Pts',(-4.31864929275468,206.87379055128,-6.1366869496822));
#1210=CARTESIAN_POINT('Ctrl Pts',(-4.19224477495804,206.809155844927,-6.22185744482189));
#1211=CARTESIAN_POINT('Ctrl Pts',(-4.06099995549939,206.74204613624,-6.31028930194741));
#1212=CARTESIAN_POINT('Ctrl Pts',(-3.92675391456938,206.674628800622,-6.39469921942834));
#1213=CARTESIAN_POINT('Ctrl Pts',(-3.78989358567387,206.607105531561,-6.47480755900256));
#1214=CARTESIAN_POINT('Ctrl Pts',(-3.65809843300235,206.542081286575,-6.55195110329805));
#1215=CARTESIAN_POINT('Ctrl Pts',(-3.52387957064261,206.476959054234,-6.62510554744148));
#1216=CARTESIAN_POINT('Ctrl Pts',(-3.38761165659103,206.411920847683,-6.69406554949809));
#1217=CARTESIAN_POINT('Ctrl Pts',(-3.25136744669109,206.346893954693,-6.76301355578624));
#1218=CARTESIAN_POINT('Ctrl Pts',(-3.11307538411878,206.281951283189,-6.82776836820748));
#1219=CARTESIAN_POINT('Ctrl Pts',(-2.97313145734166,206.217273190525,-6.88817215625554));
#1220=CARTESIAN_POINT('Ctrl Pts',(-2.8331499774231,206.152577741871,-6.94859215330993));
#1221=CARTESIAN_POINT('Ctrl Pts',(-2.69151625970553,206.088147231022,-7.00465866845592));
#1222=CARTESIAN_POINT('Ctrl Pts',(-2.54864063859631,206.02415727582,-7.05626368640968));
#1223=CARTESIAN_POINT('Ctrl Pts',(-2.53215775104539,206.016775056041,-7.06221711430306));
#1224=CARTESIAN_POINT('Ctrl Pts',(-2.51565834512647,206.009398692253,-7.06811121908845));
#1225=CARTESIAN_POINT('Ctrl Pts',(-2.49914305799788,206.002028447915,-7.07394587853976));
#1226=CARTESIAN_POINT('Ctrl Pts',(-2.35598079299498,205.938139708658,-7.12452344682942));
#1227=CARTESIAN_POINT('Ctrl Pts',(-2.21093899485714,205.87379055128,-7.1708721361652));
#1228=CARTESIAN_POINT('Ctrl Pts',(-2.06440202410006,205.809155844927,-7.21281294639894));
#1229=CARTESIAN_POINT('Ctrl Pts',(-1.91225383662799,205.74204613624,-7.25635976072986));
#1230=CARTESIAN_POINT('Ctrl Pts',(-1.75849416561927,205.674628800623,-7.29515405471511));
#1231=CARTESIAN_POINT('Ctrl Pts',(-1.60357741968129,205.607105531561,-7.32904944559231));
#1232=CARTESIAN_POINT('Ctrl Pts',(-1.45439411472333,205.542081286575,-7.36169037413289));
#1233=CARTESIAN_POINT('Ctrl Pts',(-1.30413842461202,205.476959054234,-7.38978847549662));
#1234=CARTESIAN_POINT('Ctrl Pts',(-1.15323012442371,205.411920847683,-7.41326423358633));
#1235=CARTESIAN_POINT('Ctrl Pts',(-1.00234807511963,205.346893954693,-7.43673590800795));
#1236=CARTESIAN_POINT('Ctrl Pts',(-0.850814170352673,205.281951283189,-7.45558679680064));
#1237=CARTESIAN_POINT('Ctrl Pts',(-0.699053789843954,205.217273190525,-7.46978916139896));
#1238=CARTESIAN_POINT('Ctrl Pts',(-0.547252685316885,205.152577741871,-7.48399533711949));
#1239=CARTESIAN_POINT('Ctrl Pts',(-0.39522550915898,205.088147231022,-7.49355053594382));
#1240=CARTESIAN_POINT('Ctrl Pts',(-0.243395891140606,205.02415727582,-7.49847882953766));
#1241=CARTESIAN_POINT('Ctrl Pts',(-0.225880023133996,205.016775056041,-7.49904738356035));
#1242=CARTESIAN_POINT('Ctrl Pts',(-0.208366777074381,205.009398692253,-7.49955441349818));
#1243=CARTESIAN_POINT('Ctrl Pts',(-0.190856796705286,205.002028447915,-7.5));
#1244=CARTESIAN_POINT('Ctrl Pts',(-0.0390720635510205,204.938139708658,
-7.50386255306115));
#1245=CARTESIAN_POINT('Ctrl Pts',(0.113193416374905,204.87379055128,-7.50312239555638));
#1246=CARTESIAN_POINT('Ctrl Pts',(0.265518780411678,204.809155844927,-7.49772806215972));
#1247=CARTESIAN_POINT('Ctrl Pts',(0.42367701122863,204.74204613624,-7.49212716810082));
#1248=CARTESIAN_POINT('Ctrl Pts',(0.581899244411101,204.674628800623,-7.48150838279936));
#1249=CARTESIAN_POINT('Ctrl Pts',(0.739708076930687,204.607105531561,-7.46587290795739));
#1250=CARTESIAN_POINT('Ctrl Pts',(0.891676432865158,204.542081286575,-7.45081609923475));
#1251=CARTESIAN_POINT('Ctrl Pts',(1.04326087688753,204.476959054234,-7.43110741988623));
#1252=CARTESIAN_POINT('Ctrl Pts',(1.19403760735073,204.411920847682,-7.40680096324187));
#1253=CARTESIAN_POINT('Ctrl Pts',(1.34478810981601,204.346893954693,-7.38249873476782));
#1254=CARTESIAN_POINT('Ctrl Pts',(1.49473066238024,204.281951283188,-7.35360044359504));
#1255=CARTESIAN_POINT('Ctrl Pts',(1.64345213319964,204.217273190525,-7.32021115834305));
#1256=CARTESIAN_POINT('Ctrl Pts',(1.79221351256366,204.15257774187,-7.28681291326991));
#1257=CARTESIAN_POINT('Ctrl Pts',(1.93975266792397,204.088147231022,-7.24892146633662));
#1258=CARTESIAN_POINT('Ctrl Pts',(2.08567414198074,204.024157275819,-7.20669061985607));
#1259=CARTESIAN_POINT('Ctrl Pts',(2.1025084152417,204.016775056041,-7.20181864597909));
#1260=CARTESIAN_POINT('Ctrl Pts',(2.1193211828951,204.009398692253,-7.19688896944649));
#1261=CARTESIAN_POINT('Ctrl Pts',(2.13611185762632,204.002028447915,-7.19190186588755));
#1262=CARTESIAN_POINT('Ctrl Pts',(2.28166131170441,203.938139708658,-7.14867131011454));
#1263=CARTESIAN_POINT('Ctrl Pts',(2.42624566734732,203.87379055128,-7.10091475754277));
#1264=CARTESIAN_POINT('Ctrl Pts',(2.56944875671865,203.809155844927,-7.04871331545308));
#1265=CARTESIAN_POINT('Ctrl Pts',(2.71813540129493,203.74204613624,-6.99451296753857));
#1266=CARTESIAN_POINT('Ctrl Pts',(2.86533230206809,203.674628800623,-6.93552054364115));
#1267=CARTESIAN_POINT('Ctrl Pts',(3.01058579312348,203.607105531561,-6.87188471229631));
#1268=CARTESIAN_POINT('Ctrl Pts',(3.15046347852877,203.542081286575,-6.81060403165528));
#1269=CARTESIAN_POINT('Ctrl Pts',(3.28853853492937,203.476959054234,-6.74501779444775));
#1270=CARTESIAN_POINT('Ctrl Pts',(3.42442461876546,203.411920847683,-6.67530840839894));
#1271=CARTESIAN_POINT('Ctrl Pts',(3.56028706487072,203.346893954693,-6.60561114847562));
#1272=CARTESIAN_POINT('Ctrl Pts',(3.69396084347661,203.281951283188,-6.53179244342338));
#1273=CARTESIAN_POINT('Ctrl Pts',(3.82508551084001,203.217273190525,-6.45407988419809));
#1274=CARTESIAN_POINT('Ctrl Pts',(3.95624536474729,203.15257774187,-6.37634647125832));
#1275=CARTESIAN_POINT('Ctrl Pts',(4.08485433881753,203.088147231021,-6.29471745739851));
#1276=CARTESIAN_POINT('Ctrl Pts',(4.21058385833727,203.024157275819,-6.20946132033675));
#1277=CARTESIAN_POINT('Ctrl Pts',(4.22508868089501,203.016775056041,-6.19962572130827));
#1278=CARTESIAN_POINT('Ctrl Pts',(4.23955521930334,203.009398692253,-6.18974188939137));
#1279=CARTESIAN_POINT('Ctrl Pts',(4.25398300016701,203.002028447915,-6.17981026821526));
#1280=CARTESIAN_POINT('Ctrl Pts',(4.37904978050104,202.938139708658,-6.09371831161216));
#1281=CARTESIAN_POINT('Ctrl Pts',(4.50180008775212,202.87379055128,-6.00362010807857));
#1282=CARTESIAN_POINT('Ctrl Pts',(4.62186318631574,202.809155844927,-5.90972139815643));
#1283=CARTESIAN_POINT('Ctrl Pts',(4.74652375991944,202.74204613624,-5.81222710407621));
#1284=CARTESIAN_POINT('Ctrl Pts',(4.86828667005455,202.674628800622,-5.71063563105829));
#1285=CARTESIAN_POINT('Ctrl Pts',(4.98676639590066,202.607105531561,-5.60522856175951));
#1286=CARTESIAN_POINT('Ctrl Pts',(5.10086120834481,202.542081286575,-5.50372258918869));
#1287=CARTESIAN_POINT('Ctrl Pts',(5.21191112857829,202.476959054234,-5.39867883198603));
#1288=CARTESIAN_POINT('Ctrl Pts',(5.319605089128,202.411920847683,-5.29039015693286));
#1289=CARTESIAN_POINT('Ctrl Pts',(5.42728031603811,202.346893954693,-5.1821203189714));
#1290=CARTESIAN_POINT('Ctrl Pts',(5.53160039987475,202.281951283188,-5.07060708921589));
#1291=CARTESIAN_POINT('Ctrl Pts',(5.6322928677404,202.217273190525,-4.95617830277011));
#1292=CARTESIAN_POINT('Ctrl Pts',(5.73301235584613,202.152577741871,-4.84171881002279));
#1293=CARTESIAN_POINT('Ctrl Pts',(5.83010200617296,202.088147231022,-4.72434264585582));
#1294=CARTESIAN_POINT('Ctrl Pts',(5.92333228977606,202.024157275819,-4.60440668292288));
#1295=CARTESIAN_POINT('Ctrl Pts',(5.93408782853791,202.016775056041,-4.59057023570412));
#1296=CARTESIAN_POINT('Ctrl Pts',(5.94479205212776,202.009398692253,-4.57669974673532));
#1297=CARTESIAN_POINT('Ctrl Pts',(5.95544464740895,202.002028447915,-4.56279578422009));
#1298=CARTESIAN_POINT('Ctrl Pts',(6.04778634614835,201.938139708658,-4.44226970733712));
#1299=CARTESIAN_POINT('Ctrl Pts',(6.13668694968221,201.87379055128,-4.31864929275467));
#1300=CARTESIAN_POINT('Ctrl Pts',(6.22185744482191,201.809155844927,-4.19224477495801));
#1301=CARTESIAN_POINT('Ctrl Pts',(6.31028930194743,201.74204613624,-4.06099995549936));
#1302=CARTESIAN_POINT('Ctrl Pts',(6.39469921942835,201.674628800622,-3.92675391456936));
#1303=CARTESIAN_POINT('Ctrl Pts',(6.47480755900257,201.607105531561,-3.78989358567385));
#1304=CARTESIAN_POINT('Ctrl Pts',(6.55195110329815,201.542081286575,-3.65809843300218));
#1305=CARTESIAN_POINT('Ctrl Pts',(6.62510554744167,201.476959054234,-3.52387957064226));
#1306=CARTESIAN_POINT('Ctrl Pts',(6.69406554949835,201.411920847682,-3.38761165659051));
#1307=CARTESIAN_POINT('Ctrl Pts',(6.76301355578675,201.346893954693,-3.25136744669006));
#1308=CARTESIAN_POINT('Ctrl Pts',(6.8277683682082,201.281951283188,-3.11307538411724));
#1309=CARTESIAN_POINT('Ctrl Pts',(6.88817215625643,201.217273190524,-2.97313145733959));
#1310=CARTESIAN_POINT('Ctrl Pts',(6.94859215331078,201.15257774187,-2.83314997742101));
#1311=CARTESIAN_POINT('Ctrl Pts',(7.00465866845674,201.088147231021,-2.69151625970341));
#1312=CARTESIAN_POINT('Ctrl Pts',(7.05626368641046,201.024157275819,-2.54864063859417));
#1313=CARTESIAN_POINT('Ctrl Pts',(7.06221711430357,201.016775056041,-2.53215775104397));
#1314=CARTESIAN_POINT('Ctrl Pts',(7.0681112190887,201.009398692253,-2.51565834512576));
#1315=CARTESIAN_POINT('Ctrl Pts',(7.07394587853975,201.002028447915,-2.49914305799789));
#1316=CARTESIAN_POINT('Ctrl Pts',(7.12452344682944,200.938139708658,-2.35598079299493));
#1317=CARTESIAN_POINT('Ctrl Pts',(7.17087213616524,200.87379055128,-2.21093899485702));
#1318=CARTESIAN_POINT('Ctrl Pts',(7.21281294639899,200.809155844927,-2.06440202409988));
#1319=CARTESIAN_POINT('Ctrl Pts',(7.25635976072991,200.74204613624,-1.91225383662782));
#1320=CARTESIAN_POINT('Ctrl Pts',(7.29515405471514,200.674628800622,-1.75849416561912));
#1321=CARTESIAN_POINT('Ctrl Pts',(7.32904944559233,200.607105531561,-1.60357741968116));
#1322=CARTESIAN_POINT('Ctrl Pts',(7.36169037413292,200.542081286575,-1.45439411472321));
#1323=CARTESIAN_POINT('Ctrl Pts',(7.38978847549664,200.476959054234,-1.30413842461191));
#1324=CARTESIAN_POINT('Ctrl Pts',(7.41326423358634,200.411920847683,-1.15323012442361));
#1325=CARTESIAN_POINT('Ctrl Pts',(7.43673590800806,200.346893954693,-1.00234807511895));
#1326=CARTESIAN_POINT('Ctrl Pts',(7.4555867968008,200.281951283188,-0.850814170351404));
#1327=CARTESIAN_POINT('Ctrl Pts',(7.46978916139914,200.217273190525,-0.699053789842093));
#1328=CARTESIAN_POINT('Ctrl Pts',(7.48399533711963,200.15257774187,-0.547252685315009));
#1329=CARTESIAN_POINT('Ctrl Pts',(7.49355053594392,200.088147231021,-0.395225509157083));
#1330=CARTESIAN_POINT('Ctrl Pts',(7.49847882953772,200.024157275819,-0.243395891138698));
#1331=CARTESIAN_POINT('Ctrl Pts',(7.49904738356038,200.016775056041,-0.225880023132722));
#1332=CARTESIAN_POINT('Ctrl Pts',(7.4995544134982,200.009398692253,-0.208366777073748));
#1333=CARTESIAN_POINT('Ctrl Pts',(7.5,200.002028447915,-0.190856796705287));
#1334=CARTESIAN_POINT('Ctrl Pts',(7.50386255306115,199.938139708658,-0.0390720635509912));
#1335=CARTESIAN_POINT('Ctrl Pts',(7.50312239555638,199.87379055128,0.113193416374972));
#1336=CARTESIAN_POINT('Ctrl Pts',(7.49772806215971,199.809155844927,0.265518780411775));
#1337=CARTESIAN_POINT('Ctrl Pts',(7.49212716810081,199.74204613624,0.423677011228717));
#1338=CARTESIAN_POINT('Ctrl Pts',(7.48150838279936,199.674628800623,0.581899244411163));
#1339=CARTESIAN_POINT('Ctrl Pts',(7.46587290795738,199.607105531561,0.73970807693074));
#1340=CARTESIAN_POINT('Ctrl Pts',(7.4508160992348,199.542081286575,0.891676432864664));
#1341=CARTESIAN_POINT('Ctrl Pts',(7.43110741988637,199.476959054234,1.04326087688649));
#1342=CARTESIAN_POINT('Ctrl Pts',(7.40680096324213,199.411920847683,1.19403760734915));
#1343=CARTESIAN_POINT('Ctrl Pts',(7.38249873476819,199.346893954694,1.34478810981391));
#1344=CARTESIAN_POINT('Ctrl Pts',(7.35360044359557,199.281951283189,1.49473066237762));
#1345=CARTESIAN_POINT('Ctrl Pts',(7.32021115834376,199.217273190526,1.64345213319651));
#1346=CARTESIAN_POINT('Ctrl Pts',(7.28681291327069,199.152577741872,1.79221351256049));
#1347=CARTESIAN_POINT('Ctrl Pts',(7.24892146633748,199.088147231023,1.93975266792075));
#1348=CARTESIAN_POINT('Ctrl Pts',(7.20669061985702,199.02415727582,2.08567414197748));
#1349=CARTESIAN_POINT('Ctrl Pts',(7.20181864597973,199.016775056042,2.10250841523952));
#1350=CARTESIAN_POINT('Ctrl Pts',(7.19688896944681,199.009398692254,2.11932118289401));
#1351=CARTESIAN_POINT('Ctrl Pts',(7.19190186588755,199.002028447915,2.13611185762632));
#1352=CARTESIAN_POINT('Ctrl Pts',(7.14867131011454,198.938139708658,2.28166131170442));
#1353=CARTESIAN_POINT('Ctrl Pts',(7.10091475754276,198.87379055128,2.42624566734735));
#1354=CARTESIAN_POINT('Ctrl Pts',(7.04871331545307,198.809155844927,2.56944875671869));
#1355=CARTESIAN_POINT('Ctrl Pts',(6.99451296753856,198.74204613624,2.71813540129497));
#1356=CARTESIAN_POINT('Ctrl Pts',(6.93552054364114,198.674628800622,2.86533230206812));
#1357=CARTESIAN_POINT('Ctrl Pts',(6.8718847122963,198.607105531561,3.0105857931235));
#1358=CARTESIAN_POINT('Ctrl Pts',(6.81060403165536,198.542081286575,3.1504634785286));
#1359=CARTESIAN_POINT('Ctrl Pts',(6.74501779444792,198.476959054234,3.288538534929));
#1360=CARTESIAN_POINT('Ctrl Pts',(6.67530840839923,198.411920847683,3.42442461876491));
#1361=CARTESIAN_POINT('Ctrl Pts',(6.60561114847646,198.346893954694,3.56028706486911));
#1362=CARTESIAN_POINT('Ctrl Pts',(6.53179244342483,198.281951283189,3.69396084347398));
#1363=CARTESIAN_POINT('Ctrl Pts',(6.45407988420023,198.217273190526,3.8250855108364));
#1364=CARTESIAN_POINT('Ctrl Pts',(6.37634647126055,198.152577741872,3.9562453647437));
#1365=CARTESIAN_POINT('Ctrl Pts',(6.29471745740083,198.088147231023,4.08485433881396));
#1366=CARTESIAN_POINT('Ctrl Pts',(6.20946132033916,198.024157275821,4.21058385833372));
#1367=CARTESIAN_POINT('Ctrl Pts',(6.19962572130989,198.016775056042,4.22508868089265));
#1368=CARTESIAN_POINT('Ctrl Pts',(6.18974188939218,198.009398692254,4.23955521930217));
#1369=CARTESIAN_POINT('Ctrl Pts',(6.17981026821526,198.002028447915,4.25398300016701));
#1370=CARTESIAN_POINT('Ctrl Pts',(6.09371831161217,197.938139708658,4.37904978050101));
#1371=CARTESIAN_POINT('Ctrl Pts',(6.0036201080786,197.87379055128,4.50180008775207));
#1372=CARTESIAN_POINT('Ctrl Pts',(5.90972139815648,197.809155844927,4.62186318631566));
#1373=CARTESIAN_POINT('Ctrl Pts',(5.81222710407627,197.74204613624,4.74652375991938));
#1374=CARTESIAN_POINT('Ctrl Pts',(5.71063563105834,197.674628800623,4.86828667005449));
#1375=CARTESIAN_POINT('Ctrl Pts',(5.60522856175956,197.607105531561,4.9867663959006));
#1376=CARTESIAN_POINT('Ctrl Pts',(5.50372258918911,197.542081286575,5.10086120834435));
#1377=CARTESIAN_POINT('Ctrl Pts',(5.39867883198685,197.476959054235,5.21191112857743));
#1378=CARTESIAN_POINT('Ctrl Pts',(5.29039015693409,197.411920847683,5.31960508912677));
#1379=CARTESIAN_POINT('Ctrl Pts',(5.18212031897387,197.346893954695,5.4272803160357));
#1380=CARTESIAN_POINT('Ctrl Pts',(5.07060708921967,197.281951283191,5.53160039987124));
#1381=CARTESIAN_POINT('Ctrl Pts',(4.95617830277527,197.217273190528,5.63229286773586));
#1382=CARTESIAN_POINT('Ctrl Pts',(4.84171881002731,197.152577741873,5.73301235584234));
#1383=CARTESIAN_POINT('Ctrl Pts',(4.72434264585968,197.088147231024,5.83010200616986));
#1384=CARTESIAN_POINT('Ctrl Pts',(4.60440668292603,197.024157275821,5.92333228977361));
#1385=CARTESIAN_POINT('Ctrl Pts',(4.59057023570623,197.016775056042,5.93408782853628));
#1386=CARTESIAN_POINT('Ctrl Pts',(4.57669974673637,197.009398692254,5.94479205212695));
#1387=CARTESIAN_POINT('Ctrl Pts',(4.56279578422009,197.002028447915,5.95544464740895));
#1388=CARTESIAN_POINT('Ctrl Pts',(4.44226970733712,196.938139708658,6.04778634614835));
#1389=CARTESIAN_POINT('Ctrl Pts',(4.31864929275467,196.87379055128,6.13668694968221));
#1390=CARTESIAN_POINT('Ctrl Pts',(4.19224477495802,196.809155844927,6.22185744482191));
#1391=CARTESIAN_POINT('Ctrl Pts',(4.06099995549936,196.74204613624,6.31028930194743));
#1392=CARTESIAN_POINT('Ctrl Pts',(3.92675391456935,196.674628800622,6.39469921942835));
#1393=CARTESIAN_POINT('Ctrl Pts',(3.78989358567384,196.607105531561,6.47480755900257));
#1394=CARTESIAN_POINT('Ctrl Pts',(3.6580984330025,196.542081286575,6.55195110329796));
#1395=CARTESIAN_POINT('Ctrl Pts',(3.52387957064293,196.476959054234,6.62510554744131));
#1396=CARTESIAN_POINT('Ctrl Pts',(3.38761165659153,196.411920847683,6.69406554949784));
#1397=CARTESIAN_POINT('Ctrl Pts',(3.25136744669109,196.346893954693,6.76301355578625));
#1398=CARTESIAN_POINT('Ctrl Pts',(3.11307538411827,196.281951283188,6.82776836820773));
#1399=CARTESIAN_POINT('Ctrl Pts',(2.97313145734063,196.217273190525,6.88817215625598));
#1400=CARTESIAN_POINT('Ctrl Pts',(2.83314997742163,196.15257774187,6.94859215331054));
#1401=CARTESIAN_POINT('Ctrl Pts',(2.69151625970362,196.088147231021,7.00465866845667));
#1402=CARTESIAN_POINT('Ctrl Pts',(2.54864063859395,196.024157275819,7.05626368641054));
#1403=CARTESIAN_POINT('Ctrl Pts',(2.53215775104383,196.016775056041,7.06221711430362));
#1404=CARTESIAN_POINT('Ctrl Pts',(2.51565834512569,196.009398692253,7.06811121908872));
#1405=CARTESIAN_POINT('Ctrl Pts',(2.49914305799789,196.002028447915,7.07394587853975));
#1406=CARTESIAN_POINT('Ctrl Pts',(2.35598079299495,195.938139708658,7.12452344682943));
#1407=CARTESIAN_POINT('Ctrl Pts',(2.21093899485708,195.87379055128,7.17087213616522));
#1408=CARTESIAN_POINT('Ctrl Pts',(2.06440202409996,195.809155844927,7.21281294639897));
#1409=CARTESIAN_POINT('Ctrl Pts',(1.9122538366279,195.74204613624,7.25635976072989));
#1410=CARTESIAN_POINT('Ctrl Pts',(1.75849416561919,195.674628800623,7.29515405471513));
#1411=CARTESIAN_POINT('Ctrl Pts',(1.60357741968122,195.607105531561,7.32904944559232));
#1412=CARTESIAN_POINT('Ctrl Pts',(1.4543941147231,195.542081286575,7.36169037413294));
#1413=CARTESIAN_POINT('Ctrl Pts',(1.30413842461163,195.476959054234,7.38978847549669));
#1414=CARTESIAN_POINT('Ctrl Pts',(1.15323012442317,195.411920847683,7.41326423358641));
#1415=CARTESIAN_POINT('Ctrl Pts',(1.00234807511844,195.346893954693,7.43673590800813));
#1416=CARTESIAN_POINT('Ctrl Pts',(0.850814170350841,195.281951283188,7.45558679680086));
#1417=CARTESIAN_POINT('Ctrl Pts',(0.69905378984147,195.217273190524,7.46978916139919));
#1418=CARTESIAN_POINT('Ctrl Pts',(0.547252685314392,195.15257774187,7.48399533711967));
#1419=CARTESIAN_POINT('Ctrl Pts',(0.395225509156497,195.088147231021,7.49355053594395));
#1420=CARTESIAN_POINT('Ctrl Pts',(0.243395891138119,195.024157275819,7.49847882953774));
#1421=CARTESIAN_POINT('Ctrl Pts',(0.225880023132343,195.016775056041,7.4990473835604));
#1422=CARTESIAN_POINT('Ctrl Pts',(0.208366777073546,195.009398692253,7.49955441349821));
#1423=CARTESIAN_POINT('Ctrl Pts',(0.190856796705285,195.002028447915,7.5));
#1424=CARTESIAN_POINT('Ctrl Pts',(0.127311648028404,194.975281229334,7.50161706980302));
#1425=CARTESIAN_POINT('Ctrl Pts',(0.0636823578853578,194.948453397593,7.50242803155527));
#1426=CARTESIAN_POINT('Ctrl Pts',(-4.06843965232862E-7,194.921557632927,
7.50242802810186));
#1427=CARTESIAN_POINT('Origin',(0.,400.,3.5527136788005E-14));
#1428=CARTESIAN_POINT('Origin',(0.,240.,0.));
#1429=CARTESIAN_POINT('Ctrl Pts',(5.38002895896315E-16,217.99585953923,
7.50000000439337));
#1430=CARTESIAN_POINT('Ctrl Pts',(-1.18775172812189,217.495912211348,7.50000000439337));
#1431=CARTESIAN_POINT('Ctrl Pts',(-2.317383311169,216.995967593475,7.13300320026677));
#1432=CARTESIAN_POINT('Ctrl Pts',(-3.44714003087638,216.495967593475,6.76596574150984));
#1433=CARTESIAN_POINT('Ctrl Pts',(-4.40818170865423,215.995967593475,6.06777834873578));
#1434=CARTESIAN_POINT('Ctrl Pts',(-5.36922338643209,215.495967593475,5.36959095596173));
#1435=CARTESIAN_POINT('Ctrl Pts',(-6.06747656688843,214.995967593475,4.40859707573286));
#1436=CARTESIAN_POINT('Ctrl Pts',(-6.76572974734476,214.495967593475,3.447603195504));
#1437=CARTESIAN_POINT('Ctrl Pts',(-7.13284454416054,213.995967593475,2.31787160445521));
#1438=CARTESIAN_POINT('Ctrl Pts',(-7.49995934097631,213.495967593475,1.18814001340642));
#1439=CARTESIAN_POINT('Ctrl Pts',(-7.5,212.995967593475,0.000256710972401669));
#1440=CARTESIAN_POINT('Ctrl Pts',(-7.50004065902369,212.495967593475,-1.18762659146162));
#1441=CARTESIAN_POINT('Ctrl Pts',(-7.13300320026677,211.995967593475,-2.317383311169));
#1442=CARTESIAN_POINT('Ctrl Pts',(-6.76596574150984,211.495967593475,-3.44714003087638));
#1443=CARTESIAN_POINT('Ctrl Pts',(-6.06777834873578,210.995967593475,-4.40818170865423));
#1444=CARTESIAN_POINT('Ctrl Pts',(-5.36959095596173,210.495967593475,-5.36922338643209));
#1445=CARTESIAN_POINT('Ctrl Pts',(-4.40859707573286,209.995967593475,-6.06747656688843));
#1446=CARTESIAN_POINT('Ctrl Pts',(-3.447603195504,209.495967593475,-6.76572974734476));
#1447=CARTESIAN_POINT('Ctrl Pts',(-2.31787160445521,208.995967593475,-7.13284454416054));
#1448=CARTESIAN_POINT('Ctrl Pts',(-1.18814001340642,208.495967593475,-7.49995934097631));
#1449=CARTESIAN_POINT('Ctrl Pts',(-0.000256710972402128,207.995967593475,
-7.5));
#1450=CARTESIAN_POINT('Ctrl Pts',(1.18762659146162,207.495967593475,-7.50004065902369));
#1451=CARTESIAN_POINT('Ctrl Pts',(2.317383311169,206.995967593475,-7.13300320026677));
#1452=CARTESIAN_POINT('Ctrl Pts',(3.44714003087638,206.495967593475,-6.76596574150984));
#1453=CARTESIAN_POINT('Ctrl Pts',(4.40818170865423,205.995967593475,-6.06777834873578));
#1454=CARTESIAN_POINT('Ctrl Pts',(5.36922338643209,205.495967593475,-5.36959095596173));
#1455=CARTESIAN_POINT('Ctrl Pts',(6.06747656688843,204.995967593475,-4.40859707573286));
#1456=CARTESIAN_POINT('Ctrl Pts',(6.76572974734476,204.495967593475,-3.447603195504));
#1457=CARTESIAN_POINT('Ctrl Pts',(7.13284454416054,203.995967593475,-2.31787160445521));
#1458=CARTESIAN_POINT('Ctrl Pts',(7.49995934097631,203.495967593475,-1.18814001340642));
#1459=CARTESIAN_POINT('Ctrl Pts',(7.5,202.995967593475,-0.000256710972402588));
#1460=CARTESIAN_POINT('Ctrl Pts',(7.50004065902369,202.495967593475,1.18762659146162));
#1461=CARTESIAN_POINT('Ctrl Pts',(7.13300320026677,201.995967593475,2.317383311169));
#1462=CARTESIAN_POINT('Ctrl Pts',(6.76596574150984,201.495967593475,3.44714003087638));
#1463=CARTESIAN_POINT('Ctrl Pts',(6.06777834873579,200.995967593475,4.40818170865423));
#1464=CARTESIAN_POINT('Ctrl Pts',(5.36959095596173,200.495967593475,5.36922338643209));
#1465=CARTESIAN_POINT('Ctrl Pts',(4.40859707573286,199.995967593475,6.06747656688843));
#1466=CARTESIAN_POINT('Ctrl Pts',(3.447603195504,199.495967593475,6.76572974734476));
#1467=CARTESIAN_POINT('Ctrl Pts',(2.31787160445521,198.995967593475,7.13284454416054));
#1468=CARTESIAN_POINT('Ctrl Pts',(1.18814001340643,198.495967593475,7.49995934097631));
#1469=CARTESIAN_POINT('Ctrl Pts',(0.00025671097240121,197.995967593475,
7.5));
#1470=CARTESIAN_POINT('Ctrl Pts',(0.000128355486237033,197.995913566499,
7.50000000439337));
#1471=CARTESIAN_POINT('Ctrl Pts',(5.38866871829646E-16,197.99585953923,
7.50000000439337));
#1472=CARTESIAN_POINT('Ctrl Pts',(-4.06843934450864E-7,234.921557632927,
7.50242802810186));
#1473=CARTESIAN_POINT('Ctrl Pts',(-0.152090385416014,234.857323985265,7.50242801985428));
#1474=CARTESIAN_POINT('Ctrl Pts',(-0.304485788638578,234.792702491972,7.49779895914527));
#1475=CARTESIAN_POINT('Ctrl Pts',(-0.456762644215501,234.72787053402,7.48851081348607));
#1476=CARTESIAN_POINT('Ctrl Pts',(-0.609070650331329,234.663025313709,7.4792207677959));
#1477=CARTESIAN_POINT('Ctrl Pts',(-0.761259533138642,234.597969762788,7.46526968655066));
#1478=CARTESIAN_POINT('Ctrl Pts',(-0.912902720439174,234.532885263597,7.44667945730601));
#1479=CARTESIAN_POINT('Ctrl Pts',(-1.06450493068721,234.467818351553,7.42809425151684));
#1480=CARTESIAN_POINT('Ctrl Pts',(-1.2155612127989,234.402722732839,7.40487246128567));
#1481=CARTESIAN_POINT('Ctrl Pts',(-1.36565093134662,234.3377801784,7.3770877621566));
#1482=CARTESIAN_POINT('Ctrl Pts',(-1.51579830432564,234.272812677376,7.34929239000448));
#1483=CARTESIAN_POINT('Ctrl Pts',(-1.66497786162574,234.207998581557,7.31693074896052));
#1484=CARTESIAN_POINT('Ctrl Pts',(-1.81278187771317,234.143517028959,7.28012693437987));
#1485=CARTESIAN_POINT('Ctrl Pts',(-1.92135204017761,234.096151789321,7.25309251248725));
#1486=CARTESIAN_POINT('Ctrl Pts',(-2.02918025203209,234.04896593395,7.22366229239563));
#1487=CARTESIAN_POINT('Ctrl Pts',(-2.13611185762633,234.002028447915,7.19190186588755));
#1488=CARTESIAN_POINT('Ctrl Pts',(-2.28166131170441,233.938139708658,7.14867131011454));
#1489=CARTESIAN_POINT('Ctrl Pts',(-2.42624566734732,233.87379055128,7.10091475754277));
#1490=CARTESIAN_POINT('Ctrl Pts',(-2.56944875671866,233.809155844927,7.04871331545308));
#1491=CARTESIAN_POINT('Ctrl Pts',(-2.71813540129493,233.74204613624,6.99451296753857));
#1492=CARTESIAN_POINT('Ctrl Pts',(-2.8653323020681,233.674628800622,6.93552054364115));
#1493=CARTESIAN_POINT('Ctrl Pts',(-3.01058579312348,233.607105531561,6.8718847122963));
#1494=CARTESIAN_POINT('Ctrl Pts',(-3.15046347852879,233.542081286575,6.81060403165527));
#1495=CARTESIAN_POINT('Ctrl Pts',(-3.28853853492939,233.476959054234,6.74501779444774));
#1496=CARTESIAN_POINT('Ctrl Pts',(-3.42442461876549,233.411920847683,6.67530840839893));
#1497=CARTESIAN_POINT('Ctrl Pts',(-3.56028706487034,233.346893954693,6.60561114847581));
#1498=CARTESIAN_POINT('Ctrl Pts',(-3.69396084347583,233.281951283188,6.5317924434238));
#1499=CARTESIAN_POINT('Ctrl Pts',(-3.82508551083885,233.217273190525,6.45407988419878));
#1500=CARTESIAN_POINT('Ctrl Pts',(-3.95624536474616,233.152577741871,6.37634647125902));
#1501=CARTESIAN_POINT('Ctrl Pts',(-4.08485433881642,233.088147231022,6.29471745739923));
#1502=CARTESIAN_POINT('Ctrl Pts',(-4.21058385833618,233.024157275819,6.20946132033749));
#1503=CARTESIAN_POINT('Ctrl Pts',(-4.22508868089429,233.016775056041,6.19962572130877));
#1504=CARTESIAN_POINT('Ctrl Pts',(-4.23955521930298,233.009398692253,6.18974188939162));
#1505=CARTESIAN_POINT('Ctrl Pts',(-4.25398300016701,233.002028447915,6.17981026821526));
#1506=CARTESIAN_POINT('Ctrl Pts',(-4.3790497805011,232.938139708658,6.09371831161211));
#1507=CARTESIAN_POINT('Ctrl Pts',(-4.50180008775226,232.87379055128,6.00362010807847));
#1508=CARTESIAN_POINT('Ctrl Pts',(-4.62186318631593,232.809155844927,5.90972139815627));
#1509=CARTESIAN_POINT('Ctrl Pts',(-4.74652375991963,232.74204613624,5.81222710407607));
#1510=CARTESIAN_POINT('Ctrl Pts',(-4.86828667005471,232.674628800622,5.71063563105815));
#1511=CARTESIAN_POINT('Ctrl Pts',(-4.9867663959008,232.607105531561,5.60522856175938));
#1512=CARTESIAN_POINT('Ctrl Pts',(-5.10086120834483,232.542081286575,5.50372258918868));
#1513=CARTESIAN_POINT('Ctrl Pts',(-5.21191112857818,232.476959054234,5.39867883198613));
#1514=CARTESIAN_POINT('Ctrl Pts',(-5.31960508912778,232.411920847683,5.29039015693308));
#1515=CARTESIAN_POINT('Ctrl Pts',(-5.4272803160379,232.346893954693,5.18212031897162));
#1516=CARTESIAN_POINT('Ctrl Pts',(-5.53160039987455,232.281951283189,5.07060708921611));
#1517=CARTESIAN_POINT('Ctrl Pts',(-5.63229286774021,232.217273190525,4.95617830277033));
#1518=CARTESIAN_POINT('Ctrl Pts',(-5.7330123558459,232.152577741871,4.84171881002306));
#1519=CARTESIAN_POINT('Ctrl Pts',(-5.83010200617269,232.088147231022,4.72434264585615));
#1520=CARTESIAN_POINT('Ctrl Pts',(-5.92333228977576,232.02415727582,4.60440668292327));
#1521=CARTESIAN_POINT('Ctrl Pts',(-5.9340878285377,232.016775056041,4.59057023570438));
#1522=CARTESIAN_POINT('Ctrl Pts',(-5.94479205212766,232.009398692253,4.57669974673544));
#1523=CARTESIAN_POINT('Ctrl Pts',(-5.95544464740896,232.002028447915,4.56279578422008));
#1524=CARTESIAN_POINT('Ctrl Pts',(-6.04778634614836,231.938139708658,4.44226970733711));
#1525=CARTESIAN_POINT('Ctrl Pts',(-6.13668694968222,231.87379055128,4.31864929275465));
#1526=CARTESIAN_POINT('Ctrl Pts',(-6.22185744482192,231.809155844927,4.192244774958));
#1527=CARTESIAN_POINT('Ctrl Pts',(-6.31028930194744,231.74204613624,4.06099995549935));
#1528=CARTESIAN_POINT('Ctrl Pts',(-6.39469921942836,231.674628800622,3.92675391456934));
#1529=CARTESIAN_POINT('Ctrl Pts',(-6.47480755900258,231.607105531561,3.78989358567383));
#1530=CARTESIAN_POINT('Ctrl Pts',(-6.55195110329806,231.542081286575,3.65809843300233));
#1531=CARTESIAN_POINT('Ctrl Pts',(-6.62510554744149,231.476959054234,3.52387957064259));
#1532=CARTESIAN_POINT('Ctrl Pts',(-6.6940655494981,231.411920847683,3.38761165659102));
#1533=CARTESIAN_POINT('Ctrl Pts',(-6.76301355578627,231.346893954693,3.25136744669103));
#1534=CARTESIAN_POINT('Ctrl Pts',(-6.82776836820753,231.281951283188,3.11307538411867));
#1535=CARTESIAN_POINT('Ctrl Pts',(-6.8881721562556,231.217273190525,2.97313145734151));
#1536=CARTESIAN_POINT('Ctrl Pts',(-6.94859215330999,231.152577741871,2.83314997742295));
#1537=CARTESIAN_POINT('Ctrl Pts',(-7.00465866845598,231.088147231022,2.69151625970537));
#1538=CARTESIAN_POINT('Ctrl Pts',(-7.05626368640974,231.024157275819,2.54864063859615));
#1539=CARTESIAN_POINT('Ctrl Pts',(-7.06221711430309,231.016775056041,2.53215775104529));
#1540=CARTESIAN_POINT('Ctrl Pts',(-7.06811121908846,231.009398692253,2.51565834512643));
#1541=CARTESIAN_POINT('Ctrl Pts',(-7.07394587853975,231.002028447915,2.49914305799789));
#1542=CARTESIAN_POINT('Ctrl Pts',(-7.12452344682943,230.938139708658,2.35598079299495));
#1543=CARTESIAN_POINT('Ctrl Pts',(-7.17087213616522,230.87379055128,2.21093899485707));
#1544=CARTESIAN_POINT('Ctrl Pts',(-7.21281294639897,230.809155844927,2.06440202409995));
#1545=CARTESIAN_POINT('Ctrl Pts',(-7.25635976072989,230.74204613624,1.91225383662789));
#1546=CARTESIAN_POINT('Ctrl Pts',(-7.29515405471513,230.674628800623,1.75849416561917));
#1547=CARTESIAN_POINT('Ctrl Pts',(-7.32904944559233,230.607105531561,1.6035774196812));
#1548=CARTESIAN_POINT('Ctrl Pts',(-7.36169037413292,230.542081286575,1.45439411472321));
#1549=CARTESIAN_POINT('Ctrl Pts',(-7.38978847549665,230.476959054234,1.30413842461186));
#1550=CARTESIAN_POINT('Ctrl Pts',(-7.41326423358636,230.411920847683,1.15323012442351));
#1551=CARTESIAN_POINT('Ctrl Pts',(-7.43673590800799,230.346893954693,1.00234807511941));
#1552=CARTESIAN_POINT('Ctrl Pts',(-7.45558679680067,230.281951283188,0.850814170352427));
#1553=CARTESIAN_POINT('Ctrl Pts',(-7.46978916139899,230.217273190525,0.699053789843682));
#1554=CARTESIAN_POINT('Ctrl Pts',(-7.48399533711951,230.152577741871,0.547252685316623));
#1555=CARTESIAN_POINT('Ctrl Pts',(-7.49355053594384,230.088147231022,0.395225509158728));
#1556=CARTESIAN_POINT('Ctrl Pts',(-7.49847882953767,230.02415727582,0.243395891140365));
#1557=CARTESIAN_POINT('Ctrl Pts',(-7.49904738356035,230.016775056041,0.225880023133833));
#1558=CARTESIAN_POINT('Ctrl Pts',(-7.49955441349819,230.009398692253,0.208366777074296));
#1559=CARTESIAN_POINT('Ctrl Pts',(-7.5,230.002028447915,0.19085679670528));
#1560=CARTESIAN_POINT('Ctrl Pts',(-7.50386255306115,229.938139708658,0.0390720635509798));
#1561=CARTESIAN_POINT('Ctrl Pts',(-7.50312239555638,229.87379055128,-0.113193416374988));
#1562=CARTESIAN_POINT('Ctrl Pts',(-7.49772806215971,229.809155844927,-0.265518780411795));
#1563=CARTESIAN_POINT('Ctrl Pts',(-7.49212716810081,229.74204613624,-0.423677011228737));
#1564=CARTESIAN_POINT('Ctrl Pts',(-7.48150838279935,229.674628800622,-0.581899244411182));
#1565=CARTESIAN_POINT('Ctrl Pts',(-7.46587290795738,229.607105531561,-0.739708076930759));
#1566=CARTESIAN_POINT('Ctrl Pts',(-7.4508160992348,229.542081286575,-0.891676432864674));
#1567=CARTESIAN_POINT('Ctrl Pts',(-7.43110741988637,229.476959054234,-1.0432608768865));
#1568=CARTESIAN_POINT('Ctrl Pts',(-7.40680096324213,229.411920847683,-1.19403760734915));
#1569=CARTESIAN_POINT('Ctrl Pts',(-7.38249873476809,229.346893954693,-1.34478810981454));
#1570=CARTESIAN_POINT('Ctrl Pts',(-7.35360044359533,229.281951283189,-1.49473066237887));
#1571=CARTESIAN_POINT('Ctrl Pts',(-7.32021115834334,229.217273190525,-1.64345213319836));
#1572=CARTESIAN_POINT('Ctrl Pts',(-7.28681291327022,229.152577741871,-1.79221351256241));
#1573=CARTESIAN_POINT('Ctrl Pts',(-7.24892146633694,229.088147231022,-1.93975266792275));
#1574=CARTESIAN_POINT('Ctrl Pts',(-7.20669061985642,229.02415727582,-2.08567414197955));
#1575=CARTESIAN_POINT('Ctrl Pts',(-7.20181864597933,229.016775056041,-2.1025084152409));
#1576=CARTESIAN_POINT('Ctrl Pts',(-7.19688896944661,229.009398692253,-2.1193211828947));
#1577=CARTESIAN_POINT('Ctrl Pts',(-7.19190186588755,229.002028447915,-2.13611185762632));
#1578=CARTESIAN_POINT('Ctrl Pts',(-7.14867131011454,228.938139708658,-2.28166131170441));
#1579=CARTESIAN_POINT('Ctrl Pts',(-7.10091475754277,228.87379055128,-2.42624566734733));
#1580=CARTESIAN_POINT('Ctrl Pts',(-7.04871331545307,228.809155844927,-2.56944875671868));
#1581=CARTESIAN_POINT('Ctrl Pts',(-6.99451296753857,228.74204613624,-2.71813540129495));
#1582=CARTESIAN_POINT('Ctrl Pts',(-6.93552054364114,228.674628800622,-2.86533230206812));
#1583=CARTESIAN_POINT('Ctrl Pts',(-6.8718847122963,228.607105531561,-3.0105857931235));
#1584=CARTESIAN_POINT('Ctrl Pts',(-6.81060403165529,228.542081286575,-3.15046347852874));
#1585=CARTESIAN_POINT('Ctrl Pts',(-6.74501779444778,228.476959054234,-3.2885385349293));
#1586=CARTESIAN_POINT('Ctrl Pts',(-6.675308408399,228.411920847683,-3.42442461876534));
#1587=CARTESIAN_POINT('Ctrl Pts',(-6.60561114847594,228.346893954693,-3.5602870648701));
#1588=CARTESIAN_POINT('Ctrl Pts',(-6.53179244342398,228.281951283189,-3.69396084347551));
#1589=CARTESIAN_POINT('Ctrl Pts',(-6.45407988419902,228.217273190525,-3.82508551083845));
#1590=CARTESIAN_POINT('Ctrl Pts',(-6.37634647125928,228.152577741871,-3.95624536474574));
#1591=CARTESIAN_POINT('Ctrl Pts',(-6.29471745739952,228.088147231022,-4.08485433881598));
#1592=CARTESIAN_POINT('Ctrl Pts',(-6.2094613203378,228.02415727582,-4.21058385833573));
#1593=CARTESIAN_POINT('Ctrl Pts',(-6.19962572130897,228.016775056041,-4.22508868089399));
#1594=CARTESIAN_POINT('Ctrl Pts',(-6.18974188939172,228.009398692253,-4.23955521930283));
#1595=CARTESIAN_POINT('Ctrl Pts',(-6.17981026821526,228.002028447915,-4.25398300016701));
#1596=CARTESIAN_POINT('Ctrl Pts',(-6.09371831161215,227.938139708658,-4.37904978050104));
#1597=CARTESIAN_POINT('Ctrl Pts',(-6.00362010807856,227.87379055128,-4.50180008775213));
#1598=CARTESIAN_POINT('Ctrl Pts',(-5.90972139815641,227.809155844927,-4.62186318631575));
#1599=CARTESIAN_POINT('Ctrl Pts',(-5.8122271040762,227.74204613624,-4.74652375991946));
#1600=CARTESIAN_POINT('Ctrl Pts',(-5.71063563105828,227.674628800622,-4.86828667005456));
#1601=CARTESIAN_POINT('Ctrl Pts',(-5.6052285617595,227.607105531561,-4.98676639590066));
#1602=CARTESIAN_POINT('Ctrl Pts',(-5.50372258918886,227.542081286575,-5.10086120834462));
#1603=CARTESIAN_POINT('Ctrl Pts',(-5.39867883198638,227.476959054234,-5.21191112857791));
#1604=CARTESIAN_POINT('Ctrl Pts',(-5.29039015693341,227.411920847683,-5.31960508912745));
#1605=CARTESIAN_POINT('Ctrl Pts',(-5.18212031897197,227.346893954694,-5.42728031603756));
#1606=CARTESIAN_POINT('Ctrl Pts',(-5.07060708921648,227.281951283189,-5.5316003998742));
#1607=CARTESIAN_POINT('Ctrl Pts',(-4.95617830277073,227.217273190526,-5.63229286773986));
#1608=CARTESIAN_POINT('Ctrl Pts',(-4.84171881002346,227.152577741871,-5.73301235584555));
#1609=CARTESIAN_POINT('Ctrl Pts',(-4.72434264585657,227.088147231022,-5.83010200617235));
#1610=CARTESIAN_POINT('Ctrl Pts',(-4.60440668292369,227.02415727582,-5.92333228977543));
#1611=CARTESIAN_POINT('Ctrl Pts',(-4.59057023570467,227.016775056041,-5.93408782853748));
#1612=CARTESIAN_POINT('Ctrl Pts',(-4.57669974673559,227.009398692253,-5.94479205212755));
#1613=CARTESIAN_POINT('Ctrl Pts',(-4.56279578422009,227.002028447915,-5.95544464740895));
#1614=CARTESIAN_POINT('Ctrl Pts',(-4.44226970733717,226.938139708658,-6.04778634614832));
#1615=CARTESIAN_POINT('Ctrl Pts',(-4.31864929275475,226.87379055128,-6.13668694968215));
#1616=CARTESIAN_POINT('Ctrl Pts',(-4.19224477495815,226.809155844927,-6.22185744482182));
#1617=CARTESIAN_POINT('Ctrl Pts',(-4.06099995549949,226.74204613624,-6.31028930194735));
#1618=CARTESIAN_POINT('Ctrl Pts',(-3.92675391456947,226.674628800623,-6.39469921942828));
#1619=CARTESIAN_POINT('Ctrl Pts',(-3.78989358567395,226.607105531561,-6.47480755900251));
#1620=CARTESIAN_POINT('Ctrl Pts',(-3.65809843300246,226.542081286575,-6.55195110329799));
#1621=CARTESIAN_POINT('Ctrl Pts',(-3.52387957064274,226.476959054234,-6.62510554744141));
#1622=CARTESIAN_POINT('Ctrl Pts',(-3.38761165659118,226.411920847683,-6.69406554949802));
#1623=CARTESIAN_POINT('Ctrl Pts',(-3.25136744669125,226.346893954693,-6.76301355578616));
#1624=CARTESIAN_POINT('Ctrl Pts',(-3.11307538411895,226.281951283189,-6.8277683682074));
#1625=CARTESIAN_POINT('Ctrl Pts',(-2.97313145734185,226.217273190525,-6.88817215625545));
#1626=CARTESIAN_POINT('Ctrl Pts',(-2.83314997742316,226.152577741871,-6.94859215330991));
#1627=CARTESIAN_POINT('Ctrl Pts',(-2.69151625970544,226.088147231022,-7.00465866845596));
#1628=CARTESIAN_POINT('Ctrl Pts',(-2.54864063859608,226.024157275819,-7.05626368640977));
#1629=CARTESIAN_POINT('Ctrl Pts',(-2.53215775104524,226.016775056041,-7.06221711430311));
#1630=CARTESIAN_POINT('Ctrl Pts',(-2.5156583451264,226.009398692253,-7.06811121908847));
#1631=CARTESIAN_POINT('Ctrl Pts',(-2.49914305799788,226.002028447915,-7.07394587853975));
#1632=CARTESIAN_POINT('Ctrl Pts',(-2.35598079299495,225.938139708658,-7.12452344682943));
#1633=CARTESIAN_POINT('Ctrl Pts',(-2.21093899485708,225.87379055128,-7.17087213616522));
#1634=CARTESIAN_POINT('Ctrl Pts',(-2.06440202409996,225.809155844927,-7.21281294639897));
#1635=CARTESIAN_POINT('Ctrl Pts',(-1.9122538366279,225.74204613624,-7.25635976072989));
#1636=CARTESIAN_POINT('Ctrl Pts',(-1.75849416561919,225.674628800623,-7.29515405471513));
#1637=CARTESIAN_POINT('Ctrl Pts',(-1.60357741968122,225.607105531561,-7.32904944559232));
#1638=CARTESIAN_POINT('Ctrl Pts',(-1.45439411472326,225.542081286575,-7.36169037413291));
#1639=CARTESIAN_POINT('Ctrl Pts',(-1.30413842461196,225.476959054234,-7.38978847549663));
#1640=CARTESIAN_POINT('Ctrl Pts',(-1.15323012442366,225.411920847683,-7.41326423358633));
#1641=CARTESIAN_POINT('Ctrl Pts',(-1.00234807511957,225.346893954693,-7.43673590800797));
#1642=CARTESIAN_POINT('Ctrl Pts',(-0.850814170352588,225.281951283189,-7.45558679680065));
#1643=CARTESIAN_POINT('Ctrl Pts',(-0.699053789843849,225.217273190525,-7.46978916139897));
#1644=CARTESIAN_POINT('Ctrl Pts',(-0.547252685316753,225.152577741871,-7.4839953371195));
#1645=CARTESIAN_POINT('Ctrl Pts',(-0.395225509158822,225.088147231022,-7.49355053594383));
#1646=CARTESIAN_POINT('Ctrl Pts',(-0.243395891140422,225.02415727582,-7.49847882953767));
#1647=CARTESIAN_POINT('Ctrl Pts',(-0.225880023133874,225.016775056041,-7.49904738356035));
#1648=CARTESIAN_POINT('Ctrl Pts',(-0.208366777074322,225.009398692253,-7.49955441349819));
#1649=CARTESIAN_POINT('Ctrl Pts',(-0.19085679670529,225.002028447915,-7.5));
#1650=CARTESIAN_POINT('Ctrl Pts',(-0.0390720635510056,224.938139708658,
-7.50386255306115));
#1651=CARTESIAN_POINT('Ctrl Pts',(0.113193416374946,224.87379055128,-7.50312239555638));
#1652=CARTESIAN_POINT('Ctrl Pts',(0.265518780411738,224.809155844927,-7.49772806215971));
#1653=CARTESIAN_POINT('Ctrl Pts',(0.423677011228685,224.74204613624,-7.49212716810082));
#1654=CARTESIAN_POINT('Ctrl Pts',(0.581899244411136,224.674628800623,-7.48150838279936));
#1655=CARTESIAN_POINT('Ctrl Pts',(0.739708076930718,224.607105531561,-7.46587290795738));
#1656=CARTESIAN_POINT('Ctrl Pts',(0.891676432864649,224.542081286575,-7.4508160992348));
#1657=CARTESIAN_POINT('Ctrl Pts',(1.04326087688649,224.476959054234,-7.43110741988637));
#1658=CARTESIAN_POINT('Ctrl Pts',(1.19403760734915,224.411920847683,-7.40680096324213));
#1659=CARTESIAN_POINT('Ctrl Pts',(1.34478810981431,224.346893954693,-7.38249873476812));
#1660=CARTESIAN_POINT('Ctrl Pts',(1.49473066237841,224.281951283189,-7.35360044359541));
#1661=CARTESIAN_POINT('Ctrl Pts',(1.64345213319768,224.217273190526,-7.32021115834349));
#1662=CARTESIAN_POINT('Ctrl Pts',(1.79221351256174,224.152577741871,-7.28681291327038));
#1663=CARTESIAN_POINT('Ctrl Pts',(1.93975266792208,224.088147231022,-7.24892146633712));
#1664=CARTESIAN_POINT('Ctrl Pts',(2.08567414197888,224.02415727582,-7.20669061985661));
#1665=CARTESIAN_POINT('Ctrl Pts',(2.10250841524046,224.016775056041,-7.20181864597946));
#1666=CARTESIAN_POINT('Ctrl Pts',(2.11932118289448,224.009398692253,-7.19688896944667));
#1667=CARTESIAN_POINT('Ctrl Pts',(2.13611185762633,224.002028447915,-7.19190186588755));
#1668=CARTESIAN_POINT('Ctrl Pts',(2.28166131170461,223.938139708658,-7.14867131011448));
#1669=CARTESIAN_POINT('Ctrl Pts',(2.42624566734772,223.87379055128,-7.10091475754264));
#1670=CARTESIAN_POINT('Ctrl Pts',(2.56944875671925,223.809155844927,-7.04871331545287));
#1671=CARTESIAN_POINT('Ctrl Pts',(2.71813540129546,223.74204613624,-6.99451296753837));
#1672=CARTESIAN_POINT('Ctrl Pts',(2.86533230206858,223.674628800622,-6.93552054364095));
#1673=CARTESIAN_POINT('Ctrl Pts',(3.01058579312391,223.60710553156,-6.87188471229612));
#1674=CARTESIAN_POINT('Ctrl Pts',(3.1504634785292,223.542081286575,-6.81060403165508));
#1675=CARTESIAN_POINT('Ctrl Pts',(3.2885385349298,223.476959054234,-6.74501779444754));
#1676=CARTESIAN_POINT('Ctrl Pts',(3.42442461876589,223.411920847683,-6.67530840839872));
#1677=CARTESIAN_POINT('Ctrl Pts',(3.56028706487057,223.346893954693,-6.60561114847569));
#1678=CARTESIAN_POINT('Ctrl Pts',(3.69396084347589,223.281951283188,-6.53179244342376));
#1679=CARTESIAN_POINT('Ctrl Pts',(3.82508551083875,223.217273190525,-6.45407988419884));
#1680=CARTESIAN_POINT('Ctrl Pts',(3.95624536474612,223.152577741871,-6.37634647125905));
#1681=CARTESIAN_POINT('Ctrl Pts',(4.08485433881643,223.088147231022,-6.29471745739922));
#1682=CARTESIAN_POINT('Ctrl Pts',(4.21058385833625,223.024157275819,-6.20946132033745));
#1683=CARTESIAN_POINT('Ctrl Pts',(4.22508868089433,223.016775056041,-6.19962572130874));
#1684=CARTESIAN_POINT('Ctrl Pts',(4.239555219303,223.009398692253,-6.1897418893916));
#1685=CARTESIAN_POINT('Ctrl Pts',(4.253983000167,223.002028447915,-6.17981026821526));
#1686=CARTESIAN_POINT('Ctrl Pts',(4.379049780501,222.938139708658,-6.09371831161218));
#1687=CARTESIAN_POINT('Ctrl Pts',(4.50180008775205,222.87379055128,-6.00362010807862));
#1688=CARTESIAN_POINT('Ctrl Pts',(4.62186318631563,222.809155844927,-5.90972139815651));
#1689=CARTESIAN_POINT('Ctrl Pts',(4.74652375991935,222.74204613624,-5.81222710407629));
#1690=CARTESIAN_POINT('Ctrl Pts',(4.86828667005446,222.674628800623,-5.71063563105837));
#1691=CARTESIAN_POINT('Ctrl Pts',(4.98676639590057,222.607105531561,-5.60522856175958));
#1692=CARTESIAN_POINT('Ctrl Pts',(5.10086120834461,222.542081286575,-5.50372258918887));
#1693=CARTESIAN_POINT('Ctrl Pts',(5.21191112857799,222.476959054234,-5.39867883198631));
#1694=CARTESIAN_POINT('Ctrl Pts',(5.3196050891276,222.411920847683,-5.29039015693326));
#1695=CARTESIAN_POINT('Ctrl Pts',(5.42728031603795,222.346893954693,-5.18212031897158));
#1696=CARTESIAN_POINT('Ctrl Pts',(5.53160039987481,222.281951283188,-5.07060708921584));
#1697=CARTESIAN_POINT('Ctrl Pts',(5.63229286774066,222.217273190525,-4.95617830276981));
#1698=CARTESIAN_POINT('Ctrl Pts',(5.73301235584641,222.152577741871,-4.84171881002245));
#1699=CARTESIAN_POINT('Ctrl Pts',(5.83010200617326,222.088147231022,-4.72434264585545));
#1700=CARTESIAN_POINT('Ctrl Pts',(5.92333228977638,222.024157275819,-4.60440668292247));
#1701=CARTESIAN_POINT('Ctrl Pts',(5.93408782853811,222.016775056041,-4.59057023570385));
#1702=CARTESIAN_POINT('Ctrl Pts',(5.94479205212787,222.009398692253,-4.57669974673517));
#1703=CARTESIAN_POINT('Ctrl Pts',(5.95544464740896,222.002028447915,-4.56279578422009));
#1704=CARTESIAN_POINT('Ctrl Pts',(6.04778634614835,221.938139708658,-4.44226970733712));
#1705=CARTESIAN_POINT('Ctrl Pts',(6.13668694968221,221.87379055128,-4.31864929275467));
#1706=CARTESIAN_POINT('Ctrl Pts',(6.2218574448219,221.809155844927,-4.19224477495803));
#1707=CARTESIAN_POINT('Ctrl Pts',(6.31028930194743,221.74204613624,-4.06099995549937));
#1708=CARTESIAN_POINT('Ctrl Pts',(6.39469921942835,221.674628800622,-3.92675391456936));
#1709=CARTESIAN_POINT('Ctrl Pts',(6.47480755900257,221.607105531561,-3.78989358567385));
#1710=CARTESIAN_POINT('Ctrl Pts',(6.55195110329805,221.542081286575,-3.65809843300234));
#1711=CARTESIAN_POINT('Ctrl Pts',(6.62510554744149,221.476959054234,-3.5238795706426));
#1712=CARTESIAN_POINT('Ctrl Pts',(6.6940655494981,221.411920847683,-3.38761165659102));
#1713=CARTESIAN_POINT('Ctrl Pts',(6.76301355578647,221.346893954693,-3.25136744669064));
#1714=CARTESIAN_POINT('Ctrl Pts',(6.8277683682079,221.281951283188,-3.11307538411788));
#1715=CARTESIAN_POINT('Ctrl Pts',(6.88817215625612,221.217273190525,-2.9731314573403));
#1716=CARTESIAN_POINT('Ctrl Pts',(6.94859215331057,221.15257774187,-2.83314997742154));
#1717=CARTESIAN_POINT('Ctrl Pts',(7.00465866845661,221.088147231021,-2.69151625970376));
#1718=CARTESIAN_POINT('Ctrl Pts',(7.0562636864104,221.024157275819,-2.54864063859434));
#1719=CARTESIAN_POINT('Ctrl Pts',(7.06221711430353,221.016775056041,-2.53215775104408));
#1720=CARTESIAN_POINT('Ctrl Pts',(7.06811121908868,221.009398692253,-2.51565834512583));
#1721=CARTESIAN_POINT('Ctrl Pts',(7.07394587853975,221.002028447915,-2.4991430579979));
#1722=CARTESIAN_POINT('Ctrl Pts',(7.12452344682937,220.938139708658,-2.35598079299513));
#1723=CARTESIAN_POINT('Ctrl Pts',(7.17087213616511,220.87379055128,-2.21093899485743));
#1724=CARTESIAN_POINT('Ctrl Pts',(7.21281294639882,220.809155844927,-2.06440202410049));
#1725=CARTESIAN_POINT('Ctrl Pts',(7.25635976072976,220.74204613624,-1.91225383662838));
#1726=CARTESIAN_POINT('Ctrl Pts',(7.29515405471502,220.674628800623,-1.75849416561964));
#1727=CARTESIAN_POINT('Ctrl Pts',(7.32904944559223,220.607105531561,-1.60357741968163));
#1728=CARTESIAN_POINT('Ctrl Pts',(7.36169037413284,220.542081286575,-1.4543941147236));
#1729=CARTESIAN_POINT('Ctrl Pts',(7.38978847549659,220.476959054234,-1.30413842461222));
#1730=CARTESIAN_POINT('Ctrl Pts',(7.41326423358631,220.411920847683,-1.15323012442383));
#1731=CARTESIAN_POINT('Ctrl Pts',(7.43673590800786,220.346893954694,-1.00234807512029));
#1732=CARTESIAN_POINT('Ctrl Pts',(7.4555867968005,220.281951283189,-0.850814170353856));
#1733=CARTESIAN_POINT('Ctrl Pts',(7.4697891613988,220.217273190526,-0.69905378984567));
#1734=CARTESIAN_POINT('Ctrl Pts',(7.48399533711939,220.152577741872,-0.547252685318368));
#1735=CARTESIAN_POINT('Ctrl Pts',(7.49355053594376,220.088147231023,-0.395225509160228));
#1736=CARTESIAN_POINT('Ctrl Pts',(7.49847882953763,220.02415727582,-0.243395891141619));
#1737=CARTESIAN_POINT('Ctrl Pts',(7.49904738356033,220.016775056042,-0.22588002313467));
#1738=CARTESIAN_POINT('Ctrl Pts',(7.49955441349818,220.009398692253,-0.20836677707472));
#1739=CARTESIAN_POINT('Ctrl Pts',(7.5,220.002028447915,-0.190856796705287));
#1740=CARTESIAN_POINT('Ctrl Pts',(7.50386255306115,219.938139708658,-0.0390720635509813));
#1741=CARTESIAN_POINT('Ctrl Pts',(7.50312239555638,219.87379055128,0.113193416374992));
#1742=CARTESIAN_POINT('Ctrl Pts',(7.49772806215971,219.809155844927,0.265518780411804));
#1743=CARTESIAN_POINT('Ctrl Pts',(7.49212716810081,219.74204613624,0.423677011228746));
#1744=CARTESIAN_POINT('Ctrl Pts',(7.48150838279935,219.674628800622,0.581899244411192));
#1745=CARTESIAN_POINT('Ctrl Pts',(7.46587290795738,219.607105531561,0.739708076930769));
#1746=CARTESIAN_POINT('Ctrl Pts',(7.45081609923482,219.542081286575,0.891676432864501));
#1747=CARTESIAN_POINT('Ctrl Pts',(7.43110741988641,219.476959054234,1.04326087688616));
#1748=CARTESIAN_POINT('Ctrl Pts',(7.40680096324221,219.411920847683,1.19403760734863));
#1749=CARTESIAN_POINT('Ctrl Pts',(7.38249873476801,219.346893954693,1.34478810981507));
#1750=CARTESIAN_POINT('Ctrl Pts',(7.35360044359503,219.281951283188,1.49473066238045));
#1751=CARTESIAN_POINT('Ctrl Pts',(7.32021115834276,219.217273190524,1.64345213320097));
#1752=CARTESIAN_POINT('Ctrl Pts',(7.28681291326939,219.152577741869,1.79221351256585));
#1753=CARTESIAN_POINT('Ctrl Pts',(7.24892146633583,219.08814723102,1.93975266792699));
#1754=CARTESIAN_POINT('Ctrl Pts',(7.20669061985496,219.024157275817,2.08567414198458));
#1755=CARTESIAN_POINT('Ctrl Pts',(7.20181864597834,219.01677505604,2.10250841524425));
#1756=CARTESIAN_POINT('Ctrl Pts',(7.19688896944612,219.009398692252,2.11932118289636));
#1757=CARTESIAN_POINT('Ctrl Pts',(7.19190186588756,219.002028447915,2.13611185762631));
#1758=CARTESIAN_POINT('Ctrl Pts',(7.14867131011454,218.938139708658,2.28166131170442));
#1759=CARTESIAN_POINT('Ctrl Pts',(7.10091475754276,218.87379055128,2.42624566734735));
#1760=CARTESIAN_POINT('Ctrl Pts',(7.04871331545306,218.809155844927,2.56944875671871));
#1761=CARTESIAN_POINT('Ctrl Pts',(6.99451296753855,218.74204613624,2.71813540129498));
#1762=CARTESIAN_POINT('Ctrl Pts',(6.93552054364113,218.674628800622,2.86533230206815));
#1763=CARTESIAN_POINT('Ctrl Pts',(6.87188471229629,218.607105531561,3.01058579312352));
#1764=CARTESIAN_POINT('Ctrl Pts',(6.81060403165534,218.542081286575,3.15046347852863));
#1765=CARTESIAN_POINT('Ctrl Pts',(6.7450177944479,218.476959054234,3.28853853492905));
#1766=CARTESIAN_POINT('Ctrl Pts',(6.6753084083992,218.411920847683,3.42442461876496));
#1767=CARTESIAN_POINT('Ctrl Pts',(6.60561114847611,218.346893954694,3.56028706486978));
#1768=CARTESIAN_POINT('Ctrl Pts',(6.53179244342414,218.281951283189,3.69396084347523));
#1769=CARTESIAN_POINT('Ctrl Pts',(6.45407988419915,218.217273190526,3.82508551083821));
#1770=CARTESIAN_POINT('Ctrl Pts',(6.3763464712596,218.152577741871,3.95624536474522));
#1771=CARTESIAN_POINT('Ctrl Pts',(6.29471745740002,218.088147231023,4.0848543388152));
#1772=CARTESIAN_POINT('Ctrl Pts',(6.20946132033851,218.02415727582,4.21058385833468));
#1773=CARTESIAN_POINT('Ctrl Pts',(6.19962572130945,218.016775056042,4.22508868089329));
#1774=CARTESIAN_POINT('Ctrl Pts',(6.18974188939196,218.009398692253,4.23955521930249));
#1775=CARTESIAN_POINT('Ctrl Pts',(6.17981026821525,218.002028447915,4.25398300016701));
#1776=CARTESIAN_POINT('Ctrl Pts',(6.09371831161196,217.938139708658,4.37904978050132));
#1777=CARTESIAN_POINT('Ctrl Pts',(6.00362010807817,217.87379055128,4.50180008775267));
#1778=CARTESIAN_POINT('Ctrl Pts',(5.9097213981558,217.809155844927,4.62186318631654));
#1779=CARTESIAN_POINT('Ctrl Pts',(5.81222710407562,217.742046136239,4.74652375992017));
#1780=CARTESIAN_POINT('Ctrl Pts',(5.71063563105773,217.674628800622,4.8682866700552));
#1781=CARTESIAN_POINT('Ctrl Pts',(5.605228561759,217.60710553156,4.98676639590123));
#1782=CARTESIAN_POINT('Ctrl Pts',(5.50372258918827,217.542081286575,5.10086120834527));
#1783=CARTESIAN_POINT('Ctrl Pts',(5.3986788319857,217.476959054234,5.21191112857863));
#1784=CARTESIAN_POINT('Ctrl Pts',(5.29039015693262,217.411920847682,5.31960508912823));
#1785=CARTESIAN_POINT('Ctrl Pts',(5.18212031897114,217.346893954693,5.42728031603836));
#1786=CARTESIAN_POINT('Ctrl Pts',(5.07060708921561,217.281951283188,5.53160039987501));
#1787=CARTESIAN_POINT('Ctrl Pts',(4.95617830276981,217.217273190525,5.63229286774066));
#1788=CARTESIAN_POINT('Ctrl Pts',(4.84171881002289,217.152577741871,5.73301235584603));
#1789=CARTESIAN_POINT('Ctrl Pts',(4.72434264585635,217.088147231022,5.83010200617252));
#1790=CARTESIAN_POINT('Ctrl Pts',(4.60440668292385,217.02415727582,5.92333228977531));
#1791=CARTESIAN_POINT('Ctrl Pts',(4.59057023570477,217.016775056041,5.9340878285374));
#1792=CARTESIAN_POINT('Ctrl Pts',(4.57669974673563,217.009398692253,5.94479205212752));
#1793=CARTESIAN_POINT('Ctrl Pts',(4.56279578422008,217.002028447915,5.95544464740896));
#1794=CARTESIAN_POINT('Ctrl Pts',(4.44226970733684,216.938139708657,6.04778634614857));
#1795=CARTESIAN_POINT('Ctrl Pts',(4.31864929275411,216.87379055128,6.13668694968261));
#1796=CARTESIAN_POINT('Ctrl Pts',(4.19224477495716,216.809155844927,6.22185744482248));
#1797=CARTESIAN_POINT('Ctrl Pts',(4.06099995549857,216.742046136239,6.31028930194794));
#1798=CARTESIAN_POINT('Ctrl Pts',(3.92675391456862,216.674628800622,6.3946992194288));
#1799=CARTESIAN_POINT('Ctrl Pts',(3.78989358567318,216.60710553156,6.47480755900296));
#1800=CARTESIAN_POINT('Ctrl Pts',(3.65809843300166,216.542081286575,6.55195110329844));
#1801=CARTESIAN_POINT('Ctrl Pts',(3.5238795706419,216.476959054234,6.62510554744185));
#1802=CARTESIAN_POINT('Ctrl Pts',(3.38761165659031,216.411920847682,6.69406554949845));
#1803=CARTESIAN_POINT('Ctrl Pts',(3.25136744669046,216.346893954693,6.76301355578654));
#1804=CARTESIAN_POINT('Ctrl Pts',(3.11307538411824,216.281951283188,6.82776836820773));
#1805=CARTESIAN_POINT('Ctrl Pts',(2.97313145734122,216.217273190525,6.88817215625573));
#1806=CARTESIAN_POINT('Ctrl Pts',(2.83314997742261,216.152577741871,6.94859215331013));
#1807=CARTESIAN_POINT('Ctrl Pts',(2.69151625970498,216.088147231022,7.00465866845613));
#1808=CARTESIAN_POINT('Ctrl Pts',(2.54864063859571,216.024157275819,7.0562636864099));
#1809=CARTESIAN_POINT('Ctrl Pts',(2.532157751045,216.016775056041,7.0622171143032));
#1810=CARTESIAN_POINT('Ctrl Pts',(2.51565834512628,216.009398692253,7.06811121908852));
#1811=CARTESIAN_POINT('Ctrl Pts',(2.49914305799789,216.002028447915,7.07394587853975));
#1812=CARTESIAN_POINT('Ctrl Pts',(2.35598079299496,215.938139708658,7.12452344682943));
#1813=CARTESIAN_POINT('Ctrl Pts',(2.2109389948571,215.87379055128,7.17087213616521));
#1814=CARTESIAN_POINT('Ctrl Pts',(2.0644020241,215.809155844927,7.21281294639896));
#1815=CARTESIAN_POINT('Ctrl Pts',(1.91225383662793,215.74204613624,7.25635976072988));
#1816=CARTESIAN_POINT('Ctrl Pts',(1.75849416561922,215.674628800623,7.29515405471512));
#1817=CARTESIAN_POINT('Ctrl Pts',(1.60357741968125,215.607105531561,7.32904944559231));
#1818=CARTESIAN_POINT('Ctrl Pts',(1.4543941147233,215.542081286575,7.3616903741329));
#1819=CARTESIAN_POINT('Ctrl Pts',(1.30413842461201,215.476959054234,7.38978847549662));
#1820=CARTESIAN_POINT('Ctrl Pts',(1.15323012442371,215.411920847683,7.41326423358633));
#1821=CARTESIAN_POINT('Ctrl Pts',(1.00234807511962,215.346893954693,7.43673590800796));
#1822=CARTESIAN_POINT('Ctrl Pts',(0.85081417035265,215.281951283189,7.45558679680064));
#1823=CARTESIAN_POINT('Ctrl Pts',(0.699053789843915,215.217273190525,7.46978916139897));
#1824=CARTESIAN_POINT('Ctrl Pts',(0.547252685316762,215.152577741871,7.4839953371195));
#1825=CARTESIAN_POINT('Ctrl Pts',(0.395225509158773,215.088147231022,7.49355053594384));
#1826=CARTESIAN_POINT('Ctrl Pts',(0.243395891140316,215.02415727582,7.49847882953767));
#1827=CARTESIAN_POINT('Ctrl Pts',(0.225880023133805,215.016775056041,7.49904738356035));
#1828=CARTESIAN_POINT('Ctrl Pts',(0.208366777074288,215.009398692253,7.49955441349819));
#1829=CARTESIAN_POINT('Ctrl Pts',(0.190856796705293,215.002028447915,7.5));
#1830=CARTESIAN_POINT('Ctrl Pts',(0.127311648028422,214.975281229334,7.50161706980302));
#1831=CARTESIAN_POINT('Ctrl Pts',(0.0636823578853861,214.948453397593,7.50242803155527));
#1832=CARTESIAN_POINT('Ctrl Pts',(-4.068439266928E-7,214.921557632927,7.50242802810187));
#1833=CARTESIAN_POINT('Origin',(0.190856796705285,235.002028447915,28.7581985010212));
#1834=CARTESIAN_POINT('',(0.190856796705285,235.002028447915,50.0163970020424));
#1835=CARTESIAN_POINT('Ctrl Pts',(0.190856796705285,235.002028447915,7.5));
#1836=CARTESIAN_POINT('Ctrl Pts',(0.190856796705285,235.002028447915,14.5858638315753));
#1837=CARTESIAN_POINT('Ctrl Pts',(0.190856796705285,235.002028447915,21.6717276631507));
#1838=CARTESIAN_POINT('Ctrl Pts',(0.190856796705285,235.002028447915,35.8438599971648));
#1839=CARTESIAN_POINT('Ctrl Pts',(0.190856796705285,235.002028447915,42.9301284996036));
#1840=CARTESIAN_POINT('Ctrl Pts',(0.190856796705285,235.002028447915,50.0163970020424));
#1841=CARTESIAN_POINT('',(0.000256710972400845,237.995967593475,50.0163970020424));
#1842=CARTESIAN_POINT('',(0.000256710972400879,237.995967593475,50.0163970020424));
#1843=CARTESIAN_POINT('',(0.190856796705286,235.002028447915,50.0163970020424));
#1844=CARTESIAN_POINT('Origin',(0.190856796705285,175.002028447915,28.7581985010212));
#1845=CARTESIAN_POINT('',(0.190856796705285,175.002028447915,50.0163970020424));
#1846=CARTESIAN_POINT('Ctrl Pts',(0.190856796705285,175.002028447915,50.0163970020424));
#1847=CARTESIAN_POINT('Ctrl Pts',(0.190856796705285,175.002028447915,42.9301284996036));
#1848=CARTESIAN_POINT('Ctrl Pts',(0.190856796705285,175.002028447915,35.8438599971648));
#1849=CARTESIAN_POINT('Ctrl Pts',(0.190856796705285,175.002028447915,21.6717276631507));
#1850=CARTESIAN_POINT('Ctrl Pts',(0.190856796705285,175.002028447915,14.5858638315753));
#1851=CARTESIAN_POINT('Ctrl Pts',(0.190856796705285,175.002028447915,7.5));
#1852=CARTESIAN_POINT('',(0.000256710972400845,177.995967593475,50.0163970020424));
#1853=CARTESIAN_POINT('',(0.000256710972401712,177.995967593475,50.0163970020424));
#1854=CARTESIAN_POINT('',(0.00025671097240121,177.995967593475,7.5));
#1855=CARTESIAN_POINT('Ctrl Pts',(0.190856796705285,235.002028447915,7.5));
#1856=CARTESIAN_POINT('Ctrl Pts',(-0.997026505728737,234.502028447915,7.5302287469283));
#1857=CARTESIAN_POINT('Ctrl Pts',(-2.13611185762632,234.002028447915,7.19190186588755));
#1858=CARTESIAN_POINT('Ctrl Pts',(-3.27519720952391,233.502028447915,6.8535749848468));
#1859=CARTESIAN_POINT('Ctrl Pts',(-4.25398300016701,233.002028447915,6.17981026821526));
#1860=CARTESIAN_POINT('Ctrl Pts',(-5.2327687908101,232.502028447915,5.50604555158371));
#1861=CARTESIAN_POINT('Ctrl Pts',(-5.95544464740896,232.002028447915,4.56279578422009));
#1862=CARTESIAN_POINT('Ctrl Pts',(-6.67812050400781,231.502028447915,3.61954601685647));
#1863=CARTESIAN_POINT('Ctrl Pts',(-7.07394587853975,231.002028447915,2.49914305799789));
#1864=CARTESIAN_POINT('Ctrl Pts',(-7.4697712530717,230.502028447915,1.37874009913931));
#1865=CARTESIAN_POINT('Ctrl Pts',(-7.5,230.002028447915,0.190856796705286));
#1866=CARTESIAN_POINT('Ctrl Pts',(-7.5302287469283,229.502028447915,-0.997026505728736));
#1867=CARTESIAN_POINT('Ctrl Pts',(-7.19190186588755,229.002028447915,-2.13611185762632));
#1868=CARTESIAN_POINT('Ctrl Pts',(-6.8535749848468,228.502028447915,-3.27519720952391));
#1869=CARTESIAN_POINT('Ctrl Pts',(-6.17981026821526,228.002028447915,-4.25398300016701));
#1870=CARTESIAN_POINT('Ctrl Pts',(-5.50604555158371,227.502028447915,-5.2327687908101));
#1871=CARTESIAN_POINT('Ctrl Pts',(-4.56279578422009,227.002028447915,-5.95544464740895));
#1872=CARTESIAN_POINT('Ctrl Pts',(-3.61954601685647,226.502028447915,-6.67812050400781));
#1873=CARTESIAN_POINT('Ctrl Pts',(-2.49914305799789,226.002028447915,-7.07394587853975));
#1874=CARTESIAN_POINT('Ctrl Pts',(-1.37874009913931,225.502028447915,-7.4697712530717));
#1875=CARTESIAN_POINT('Ctrl Pts',(-0.190856796705286,225.002028447915,-7.5));
#1876=CARTESIAN_POINT('Ctrl Pts',(0.997026505728736,224.502028447915,-7.5302287469283));
#1877=CARTESIAN_POINT('Ctrl Pts',(2.13611185762632,224.002028447915,-7.19190186588755));
#1878=CARTESIAN_POINT('Ctrl Pts',(3.27519720952391,223.502028447915,-6.8535749848468));
#1879=CARTESIAN_POINT('Ctrl Pts',(4.25398300016701,223.002028447915,-6.17981026821526));
#1880=CARTESIAN_POINT('Ctrl Pts',(5.2327687908101,222.502028447915,-5.50604555158371));
#1881=CARTESIAN_POINT('Ctrl Pts',(5.95544464740895,222.002028447915,-4.56279578422009));
#1882=CARTESIAN_POINT('Ctrl Pts',(6.67812050400781,221.502028447915,-3.61954601685647));
#1883=CARTESIAN_POINT('Ctrl Pts',(7.07394587853975,221.002028447915,-2.49914305799789));
#1884=CARTESIAN_POINT('Ctrl Pts',(7.4697712530717,220.502028447915,-1.37874009913931));
#1885=CARTESIAN_POINT('Ctrl Pts',(7.5,220.002028447915,-0.190856796705287));
#1886=CARTESIAN_POINT('Ctrl Pts',(7.5302287469283,219.502028447915,0.997026505728735));
#1887=CARTESIAN_POINT('Ctrl Pts',(7.19190186588755,219.002028447915,2.13611185762632));
#1888=CARTESIAN_POINT('Ctrl Pts',(6.8535749848468,218.502028447915,3.27519720952391));
#1889=CARTESIAN_POINT('Ctrl Pts',(6.17981026821526,218.002028447915,4.25398300016701));
#1890=CARTESIAN_POINT('Ctrl Pts',(5.50604555158371,217.502028447915,5.2327687908101));
#1891=CARTESIAN_POINT('Ctrl Pts',(4.56279578422009,217.002028447915,5.95544464740895));
#1892=CARTESIAN_POINT('Ctrl Pts',(3.61954601685647,216.502028447915,6.67812050400781));
#1893=CARTESIAN_POINT('Ctrl Pts',(2.49914305799789,216.002028447915,7.07394587853975));
#1894=CARTESIAN_POINT('Ctrl Pts',(1.37874009913931,215.502028447915,7.4697712530717));
#1895=CARTESIAN_POINT('Ctrl Pts',(0.190856796705285,215.002028447915,7.5));
#1896=CARTESIAN_POINT('Ctrl Pts',(-0.997026505728737,214.502028447915,7.5302287469283));
#1897=CARTESIAN_POINT('Ctrl Pts',(-2.13611185762632,214.002028447915,7.19190186588755));
#1898=CARTESIAN_POINT('Ctrl Pts',(-3.27519720952391,213.502028447915,6.8535749848468));
#1899=CARTESIAN_POINT('Ctrl Pts',(-4.25398300016701,213.002028447915,6.17981026821526));
#1900=CARTESIAN_POINT('Ctrl Pts',(-5.2327687908101,212.502028447915,5.50604555158371));
#1901=CARTESIAN_POINT('Ctrl Pts',(-5.95544464740896,212.002028447915,4.56279578422009));
#1902=CARTESIAN_POINT('Ctrl Pts',(-6.67812050400781,211.502028447915,3.61954601685647));
#1903=CARTESIAN_POINT('Ctrl Pts',(-7.07394587853975,211.002028447915,2.49914305799789));
#1904=CARTESIAN_POINT('Ctrl Pts',(-7.4697712530717,210.502028447915,1.37874009913931));
#1905=CARTESIAN_POINT('Ctrl Pts',(-7.5,210.002028447915,0.190856796705286));
#1906=CARTESIAN_POINT('Ctrl Pts',(-7.5302287469283,209.502028447915,-0.997026505728736));
#1907=CARTESIAN_POINT('Ctrl Pts',(-7.19190186588755,209.002028447915,-2.13611185762632));
#1908=CARTESIAN_POINT('Ctrl Pts',(-6.8535749848468,208.502028447915,-3.27519720952391));
#1909=CARTESIAN_POINT('Ctrl Pts',(-6.17981026821526,208.002028447915,-4.25398300016701));
#1910=CARTESIAN_POINT('Ctrl Pts',(-5.50604555158371,207.502028447915,-5.2327687908101));
#1911=CARTESIAN_POINT('Ctrl Pts',(-4.56279578422009,207.002028447915,-5.95544464740895));
#1912=CARTESIAN_POINT('Ctrl Pts',(-3.61954601685647,206.502028447915,-6.67812050400781));
#1913=CARTESIAN_POINT('Ctrl Pts',(-2.49914305799789,206.002028447915,-7.07394587853975));
#1914=CARTESIAN_POINT('Ctrl Pts',(-1.37874009913931,205.502028447915,-7.4697712530717));
#1915=CARTESIAN_POINT('Ctrl Pts',(-0.190856796705286,205.002028447915,-7.5));
#1916=CARTESIAN_POINT('Ctrl Pts',(0.997026505728736,204.502028447915,-7.5302287469283));
#1917=CARTESIAN_POINT('Ctrl Pts',(2.13611185762632,204.002028447915,-7.19190186588755));
#1918=CARTESIAN_POINT('Ctrl Pts',(3.27519720952391,203.502028447915,-6.8535749848468));
#1919=CARTESIAN_POINT('Ctrl Pts',(4.25398300016701,203.002028447915,-6.17981026821526));
#1920=CARTESIAN_POINT('Ctrl Pts',(5.2327687908101,202.502028447915,-5.50604555158371));
#1921=CARTESIAN_POINT('Ctrl Pts',(5.95544464740895,202.002028447915,-4.56279578422009));
#1922=CARTESIAN_POINT('Ctrl Pts',(6.67812050400781,201.502028447915,-3.61954601685647));
#1923=CARTESIAN_POINT('Ctrl Pts',(7.07394587853975,201.002028447915,-2.49914305799789));
#1924=CARTESIAN_POINT('Ctrl Pts',(7.4697712530717,200.502028447915,-1.37874009913931));
#1925=CARTESIAN_POINT('Ctrl Pts',(7.5,200.002028447915,-0.190856796705287));
#1926=CARTESIAN_POINT('Ctrl Pts',(7.5302287469283,199.502028447915,0.997026505728735));
#1927=CARTESIAN_POINT('Ctrl Pts',(7.19190186588755,199.002028447915,2.13611185762632));
#1928=CARTESIAN_POINT('Ctrl Pts',(6.8535749848468,198.502028447915,3.27519720952391));
#1929=CARTESIAN_POINT('Ctrl Pts',(6.17981026821526,198.002028447915,4.25398300016701));
#1930=CARTESIAN_POINT('Ctrl Pts',(5.50604555158371,197.502028447915,5.2327687908101));
#1931=CARTESIAN_POINT('Ctrl Pts',(4.56279578422009,197.002028447915,5.95544464740895));
#1932=CARTESIAN_POINT('Ctrl Pts',(3.61954601685647,196.502028447915,6.67812050400781));
#1933=CARTESIAN_POINT('Ctrl Pts',(2.49914305799789,196.002028447915,7.07394587853975));
#1934=CARTESIAN_POINT('Ctrl Pts',(1.37874009913931,195.502028447915,7.4697712530717));
#1935=CARTESIAN_POINT('Ctrl Pts',(0.190856796705285,195.002028447915,7.5));
#1936=CARTESIAN_POINT('Ctrl Pts',(-0.997026505728737,194.502028447915,7.5302287469283));
#1937=CARTESIAN_POINT('Ctrl Pts',(-2.13611185762632,194.002028447915,7.19190186588755));
#1938=CARTESIAN_POINT('Ctrl Pts',(-3.27519720952391,193.502028447915,6.8535749848468));
#1939=CARTESIAN_POINT('Ctrl Pts',(-4.25398300016701,193.002028447915,6.17981026821526));
#1940=CARTESIAN_POINT('Ctrl Pts',(-5.2327687908101,192.502028447915,5.50604555158371));
#1941=CARTESIAN_POINT('Ctrl Pts',(-5.95544464740896,192.002028447915,4.56279578422009));
#1942=CARTESIAN_POINT('Ctrl Pts',(-6.67812050400781,191.502028447915,3.61954601685647));
#1943=CARTESIAN_POINT('Ctrl Pts',(-7.07394587853975,191.002028447915,2.49914305799789));
#1944=CARTESIAN_POINT('Ctrl Pts',(-7.4697712530717,190.502028447915,1.37874009913931));
#1945=CARTESIAN_POINT('Ctrl Pts',(-7.5,190.002028447915,0.190856796705286));
#1946=CARTESIAN_POINT('Ctrl Pts',(-7.5302287469283,189.502028447915,-0.997026505728736));
#1947=CARTESIAN_POINT('Ctrl Pts',(-7.19190186588755,189.002028447915,-2.13611185762632));
#1948=CARTESIAN_POINT('Ctrl Pts',(-6.8535749848468,188.502028447915,-3.27519720952391));
#1949=CARTESIAN_POINT('Ctrl Pts',(-6.17981026821526,188.002028447915,-4.25398300016701));
#1950=CARTESIAN_POINT('Ctrl Pts',(-5.50604555158371,187.502028447915,-5.2327687908101));
#1951=CARTESIAN_POINT('Ctrl Pts',(-4.56279578422009,187.002028447915,-5.95544464740895));
#1952=CARTESIAN_POINT('Ctrl Pts',(-3.61954601685647,186.502028447915,-6.67812050400781));
#1953=CARTESIAN_POINT('Ctrl Pts',(-2.49914305799789,186.002028447915,-7.07394587853975));
#1954=CARTESIAN_POINT('Ctrl Pts',(-1.37874009913931,185.502028447915,-7.4697712530717));
#1955=CARTESIAN_POINT('Ctrl Pts',(-0.190856796705286,185.002028447915,-7.5));
#1956=CARTESIAN_POINT('Ctrl Pts',(0.997026505728736,184.502028447915,-7.5302287469283));
#1957=CARTESIAN_POINT('Ctrl Pts',(2.13611185762632,184.002028447915,-7.19190186588755));
#1958=CARTESIAN_POINT('Ctrl Pts',(3.27519720952391,183.502028447915,-6.8535749848468));
#1959=CARTESIAN_POINT('Ctrl Pts',(4.25398300016701,183.002028447915,-6.17981026821526));
#1960=CARTESIAN_POINT('Ctrl Pts',(5.2327687908101,182.502028447915,-5.50604555158371));
#1961=CARTESIAN_POINT('Ctrl Pts',(5.95544464740895,182.002028447915,-4.56279578422009));
#1962=CARTESIAN_POINT('Ctrl Pts',(6.67812050400781,181.502028447915,-3.61954601685647));
#1963=CARTESIAN_POINT('Ctrl Pts',(7.07394587853975,181.002028447915,-2.49914305799789));
#1964=CARTESIAN_POINT('Ctrl Pts',(7.4697712530717,180.502028447915,-1.37874009913931));
#1965=CARTESIAN_POINT('Ctrl Pts',(7.5,180.002028447915,-0.190856796705287));
#1966=CARTESIAN_POINT('Ctrl Pts',(7.5302287469283,179.502028447915,0.997026505728735));
#1967=CARTESIAN_POINT('Ctrl Pts',(7.19190186588755,179.002028447915,2.13611185762632));
#1968=CARTESIAN_POINT('Ctrl Pts',(6.8535749848468,178.502028447915,3.27519720952391));
#1969=CARTESIAN_POINT('Ctrl Pts',(6.17981026821526,178.002028447915,4.25398300016701));
#1970=CARTESIAN_POINT('Ctrl Pts',(5.50604555158371,177.502028447915,5.2327687908101));
#1971=CARTESIAN_POINT('Ctrl Pts',(4.56279578422009,177.002028447915,5.95544464740895));
#1972=CARTESIAN_POINT('Ctrl Pts',(3.61954601685647,176.502028447915,6.67812050400781));
#1973=CARTESIAN_POINT('Ctrl Pts',(2.49914305799789,176.002028447915,7.07394587853975));
#1974=CARTESIAN_POINT('Ctrl Pts',(1.37874009913931,175.502028447915,7.4697712530717));
#1975=CARTESIAN_POINT('Ctrl Pts',(0.190856796705285,175.002028447915,7.5));
#1976=CARTESIAN_POINT('Ctrl Pts',(0.190856796705285,235.002028447915,50.0163970020424));
#1977=CARTESIAN_POINT('Ctrl Pts',(-7.73096224951301,234.502028447915,50.0466257489707));
#1978=CARTESIAN_POINT('Ctrl Pts',(-15.2744010708495,234.002028447915,47.6273982840717));
#1979=CARTESIAN_POINT('Ctrl Pts',(-22.817839892186,233.502028447915,45.2081708191727));
#1980=CARTESIAN_POINT('Ctrl Pts',(-29.2444941385794,233.002028447915,40.5762979824596));
#1981=CARTESIAN_POINT('Ctrl Pts',(-35.6711483849729,232.502028447915,35.9444251457465));
#1982=CARTESIAN_POINT('Ctrl Pts',(-40.3519323616533,232.002028447915,29.5533069226325));
#1983=CARTESIAN_POINT('Ctrl Pts',(-45.0327163383337,231.502028447915,23.1621886995185));
#1984=CARTESIAN_POINT('Ctrl Pts',(-47.5094422967239,231.002028447915,15.6374322712211));
#1985=CARTESIAN_POINT('Ctrl Pts',(-49.9861682551141,230.502028447915,8.11267584292358));
#1986=CARTESIAN_POINT('Ctrl Pts',(-50.0163970020424,230.002028447915,0.190856796705288));
#1987=CARTESIAN_POINT('Ctrl Pts',(-50.0466257489707,229.502028447915,-7.73096224951301));
#1988=CARTESIAN_POINT('Ctrl Pts',(-47.6273982840717,229.002028447915,-15.2744010708495));
#1989=CARTESIAN_POINT('Ctrl Pts',(-45.2081708191727,228.502028447915,-22.817839892186));
#1990=CARTESIAN_POINT('Ctrl Pts',(-40.5762979824596,228.002028447915,-29.2444941385794));
#1991=CARTESIAN_POINT('Ctrl Pts',(-35.9444251457465,227.502028447915,-35.6711483849729));
#1992=CARTESIAN_POINT('Ctrl Pts',(-29.5533069226325,227.002028447915,-40.3519323616533));
#1993=CARTESIAN_POINT('Ctrl Pts',(-23.1621886995185,226.502028447915,-45.0327163383337));
#1994=CARTESIAN_POINT('Ctrl Pts',(-15.6374322712211,226.002028447915,-47.5094422967239));
#1995=CARTESIAN_POINT('Ctrl Pts',(-8.11267584292359,225.502028447915,-49.9861682551141));
#1996=CARTESIAN_POINT('Ctrl Pts',(-0.190856796705292,225.002028447915,-50.0163970020424));
#1997=CARTESIAN_POINT('Ctrl Pts',(7.730962249513,224.502028447915,-50.0466257489707));
#1998=CARTESIAN_POINT('Ctrl Pts',(15.2744010708495,224.002028447915,-47.6273982840717));
#1999=CARTESIAN_POINT('Ctrl Pts',(22.817839892186,223.502028447915,-45.2081708191727));
#2000=CARTESIAN_POINT('Ctrl Pts',(29.2444941385794,223.002028447915,-40.5762979824596));
#2001=CARTESIAN_POINT('Ctrl Pts',(35.6711483849729,222.502028447915,-35.9444251457465));
#2002=CARTESIAN_POINT('Ctrl Pts',(40.3519323616533,222.002028447915,-29.5533069226325));
#2003=CARTESIAN_POINT('Ctrl Pts',(45.0327163383337,221.502028447915,-23.1621886995185));
#2004=CARTESIAN_POINT('Ctrl Pts',(47.5094422967239,221.002028447915,-15.6374322712211));
#2005=CARTESIAN_POINT('Ctrl Pts',(49.9861682551141,220.502028447915,-8.11267584292359));
#2006=CARTESIAN_POINT('Ctrl Pts',(50.0163970020424,220.002028447915,-0.190856796705295));
#2007=CARTESIAN_POINT('Ctrl Pts',(50.0466257489707,219.502028447915,7.730962249513));
#2008=CARTESIAN_POINT('Ctrl Pts',(47.6273982840717,219.002028447915,15.2744010708495));
#2009=CARTESIAN_POINT('Ctrl Pts',(45.2081708191727,218.502028447915,22.817839892186));
#2010=CARTESIAN_POINT('Ctrl Pts',(40.5762979824596,218.002028447915,29.2444941385794));
#2011=CARTESIAN_POINT('Ctrl Pts',(35.9444251457465,217.502028447915,35.6711483849729));
#2012=CARTESIAN_POINT('Ctrl Pts',(29.5533069226325,217.002028447915,40.3519323616533));
#2013=CARTESIAN_POINT('Ctrl Pts',(23.1621886995185,216.502028447915,45.0327163383337));
#2014=CARTESIAN_POINT('Ctrl Pts',(15.6374322712211,216.002028447915,47.5094422967239));
#2015=CARTESIAN_POINT('Ctrl Pts',(8.11267584292359,215.502028447915,49.9861682551141));
#2016=CARTESIAN_POINT('Ctrl Pts',(0.190856796705285,215.002028447915,50.0163970020424));
#2017=CARTESIAN_POINT('Ctrl Pts',(-7.73096224951301,214.502028447915,50.0466257489707));
#2018=CARTESIAN_POINT('Ctrl Pts',(-15.2744010708495,214.002028447915,47.6273982840717));
#2019=CARTESIAN_POINT('Ctrl Pts',(-22.817839892186,213.502028447915,45.2081708191727));
#2020=CARTESIAN_POINT('Ctrl Pts',(-29.2444941385794,213.002028447915,40.5762979824596));
#2021=CARTESIAN_POINT('Ctrl Pts',(-35.6711483849729,212.502028447915,35.9444251457465));
#2022=CARTESIAN_POINT('Ctrl Pts',(-40.3519323616533,212.002028447915,29.5533069226325));
#2023=CARTESIAN_POINT('Ctrl Pts',(-45.0327163383337,211.502028447915,23.1621886995185));
#2024=CARTESIAN_POINT('Ctrl Pts',(-47.5094422967239,211.002028447915,15.6374322712211));
#2025=CARTESIAN_POINT('Ctrl Pts',(-49.9861682551141,210.502028447915,8.11267584292358));
#2026=CARTESIAN_POINT('Ctrl Pts',(-50.0163970020424,210.002028447915,0.190856796705288));
#2027=CARTESIAN_POINT('Ctrl Pts',(-50.0466257489707,209.502028447915,-7.73096224951301));
#2028=CARTESIAN_POINT('Ctrl Pts',(-47.6273982840717,209.002028447915,-15.2744010708495));
#2029=CARTESIAN_POINT('Ctrl Pts',(-45.2081708191727,208.502028447915,-22.817839892186));
#2030=CARTESIAN_POINT('Ctrl Pts',(-40.5762979824596,208.002028447915,-29.2444941385794));
#2031=CARTESIAN_POINT('Ctrl Pts',(-35.9444251457465,207.502028447915,-35.6711483849729));
#2032=CARTESIAN_POINT('Ctrl Pts',(-29.5533069226325,207.002028447915,-40.3519323616533));
#2033=CARTESIAN_POINT('Ctrl Pts',(-23.1621886995185,206.502028447915,-45.0327163383337));
#2034=CARTESIAN_POINT('Ctrl Pts',(-15.6374322712211,206.002028447915,-47.5094422967239));
#2035=CARTESIAN_POINT('Ctrl Pts',(-8.11267584292359,205.502028447915,-49.9861682551141));
#2036=CARTESIAN_POINT('Ctrl Pts',(-0.190856796705292,205.002028447915,-50.0163970020424));
#2037=CARTESIAN_POINT('Ctrl Pts',(7.730962249513,204.502028447915,-50.0466257489707));
#2038=CARTESIAN_POINT('Ctrl Pts',(15.2744010708495,204.002028447915,-47.6273982840717));
#2039=CARTESIAN_POINT('Ctrl Pts',(22.817839892186,203.502028447915,-45.2081708191727));
#2040=CARTESIAN_POINT('Ctrl Pts',(29.2444941385794,203.002028447915,-40.5762979824596));
#2041=CARTESIAN_POINT('Ctrl Pts',(35.6711483849729,202.502028447915,-35.9444251457465));
#2042=CARTESIAN_POINT('Ctrl Pts',(40.3519323616533,202.002028447915,-29.5533069226325));
#2043=CARTESIAN_POINT('Ctrl Pts',(45.0327163383337,201.502028447915,-23.1621886995185));
#2044=CARTESIAN_POINT('Ctrl Pts',(47.5094422967239,201.002028447915,-15.6374322712211));
#2045=CARTESIAN_POINT('Ctrl Pts',(49.9861682551141,200.502028447915,-8.11267584292359));
#2046=CARTESIAN_POINT('Ctrl Pts',(50.0163970020424,200.002028447915,-0.190856796705295));
#2047=CARTESIAN_POINT('Ctrl Pts',(50.0466257489707,199.502028447915,7.730962249513));
#2048=CARTESIAN_POINT('Ctrl Pts',(47.6273982840717,199.002028447915,15.2744010708495));
#2049=CARTESIAN_POINT('Ctrl Pts',(45.2081708191727,198.502028447915,22.817839892186));
#2050=CARTESIAN_POINT('Ctrl Pts',(40.5762979824596,198.002028447915,29.2444941385794));
#2051=CARTESIAN_POINT('Ctrl Pts',(35.9444251457465,197.502028447915,35.6711483849729));
#2052=CARTESIAN_POINT('Ctrl Pts',(29.5533069226325,197.002028447915,40.3519323616533));
#2053=CARTESIAN_POINT('Ctrl Pts',(23.1621886995185,196.502028447915,45.0327163383337));
#2054=CARTESIAN_POINT('Ctrl Pts',(15.6374322712211,196.002028447915,47.5094422967239));
#2055=CARTESIAN_POINT('Ctrl Pts',(8.11267584292359,195.502028447915,49.9861682551141));
#2056=CARTESIAN_POINT('Ctrl Pts',(0.190856796705285,195.002028447915,50.0163970020424));
#2057=CARTESIAN_POINT('Ctrl Pts',(-7.73096224951301,194.502028447915,50.0466257489707));
#2058=CARTESIAN_POINT('Ctrl Pts',(-15.2744010708495,194.002028447915,47.6273982840717));
#2059=CARTESIAN_POINT('Ctrl Pts',(-22.817839892186,193.502028447915,45.2081708191727));
#2060=CARTESIAN_POINT('Ctrl Pts',(-29.2444941385794,193.002028447915,40.5762979824596));
#2061=CARTESIAN_POINT('Ctrl Pts',(-35.6711483849729,192.502028447915,35.9444251457465));
#2062=CARTESIAN_POINT('Ctrl Pts',(-40.3519323616533,192.002028447915,29.5533069226325));
#2063=CARTESIAN_POINT('Ctrl Pts',(-45.0327163383337,191.502028447915,23.1621886995185));
#2064=CARTESIAN_POINT('Ctrl Pts',(-47.5094422967239,191.002028447915,15.6374322712211));
#2065=CARTESIAN_POINT('Ctrl Pts',(-49.9861682551141,190.502028447915,8.11267584292358));
#2066=CARTESIAN_POINT('Ctrl Pts',(-50.0163970020424,190.002028447915,0.190856796705288));
#2067=CARTESIAN_POINT('Ctrl Pts',(-50.0466257489707,189.502028447915,-7.73096224951301));
#2068=CARTESIAN_POINT('Ctrl Pts',(-47.6273982840717,189.002028447915,-15.2744010708495));
#2069=CARTESIAN_POINT('Ctrl Pts',(-45.2081708191727,188.502028447915,-22.817839892186));
#2070=CARTESIAN_POINT('Ctrl Pts',(-40.5762979824596,188.002028447915,-29.2444941385794));
#2071=CARTESIAN_POINT('Ctrl Pts',(-35.9444251457465,187.502028447915,-35.6711483849729));
#2072=CARTESIAN_POINT('Ctrl Pts',(-29.5533069226325,187.002028447915,-40.3519323616533));
#2073=CARTESIAN_POINT('Ctrl Pts',(-23.1621886995185,186.502028447915,-45.0327163383337));
#2074=CARTESIAN_POINT('Ctrl Pts',(-15.6374322712211,186.002028447915,-47.5094422967239));
#2075=CARTESIAN_POINT('Ctrl Pts',(-8.11267584292359,185.502028447915,-49.9861682551141));
#2076=CARTESIAN_POINT('Ctrl Pts',(-0.190856796705292,185.002028447915,-50.0163970020424));
#2077=CARTESIAN_POINT('Ctrl Pts',(7.730962249513,184.502028447915,-50.0466257489707));
#2078=CARTESIAN_POINT('Ctrl Pts',(15.2744010708495,184.002028447915,-47.6273982840717));
#2079=CARTESIAN_POINT('Ctrl Pts',(22.817839892186,183.502028447915,-45.2081708191727));
#2080=CARTESIAN_POINT('Ctrl Pts',(29.2444941385794,183.002028447915,-40.5762979824596));
#2081=CARTESIAN_POINT('Ctrl Pts',(35.6711483849729,182.502028447915,-35.9444251457465));
#2082=CARTESIAN_POINT('Ctrl Pts',(40.3519323616533,182.002028447915,-29.5533069226325));
#2083=CARTESIAN_POINT('Ctrl Pts',(45.0327163383337,181.502028447915,-23.1621886995185));
#2084=CARTESIAN_POINT('Ctrl Pts',(47.5094422967239,181.002028447915,-15.6374322712211));
#2085=CARTESIAN_POINT('Ctrl Pts',(49.9861682551141,180.502028447915,-8.11267584292359));
#2086=CARTESIAN_POINT('Ctrl Pts',(50.0163970020424,180.002028447915,-0.190856796705295));
#2087=CARTESIAN_POINT('Ctrl Pts',(50.0466257489707,179.502028447915,7.730962249513));
#2088=CARTESIAN_POINT('Ctrl Pts',(47.6273982840717,179.002028447915,15.2744010708495));
#2089=CARTESIAN_POINT('Ctrl Pts',(45.2081708191727,178.502028447915,22.817839892186));
#2090=CARTESIAN_POINT('Ctrl Pts',(40.5762979824596,178.002028447915,29.2444941385794));
#2091=CARTESIAN_POINT('Ctrl Pts',(35.9444251457465,177.502028447915,35.6711483849729));
#2092=CARTESIAN_POINT('Ctrl Pts',(29.5533069226325,177.002028447915,40.3519323616533));
#2093=CARTESIAN_POINT('Ctrl Pts',(23.1621886995185,176.502028447915,45.0327163383337));
#2094=CARTESIAN_POINT('Ctrl Pts',(15.6374322712211,176.002028447915,47.5094422967239));
#2095=CARTESIAN_POINT('Ctrl Pts',(8.11267584292359,175.502028447915,49.9861682551141));
#2096=CARTESIAN_POINT('Ctrl Pts',(0.190856796705285,175.002028447915,50.0163970020424));
#2097=CARTESIAN_POINT('Ctrl Pts',(0.190856796705285,235.002028447915,50.0163970020424));
#2098=CARTESIAN_POINT('Ctrl Pts',(-7.73096224951301,234.502028447915,50.0466257489707));
#2099=CARTESIAN_POINT('Ctrl Pts',(-15.2744010708495,234.002028447915,47.6273982840717));
#2100=CARTESIAN_POINT('Ctrl Pts',(-22.817839892186,233.502028447915,45.2081708191727));
#2101=CARTESIAN_POINT('Ctrl Pts',(-29.2444941385794,233.002028447915,40.5762979824596));
#2102=CARTESIAN_POINT('Ctrl Pts',(-35.6711483849729,232.502028447915,35.9444251457465));
#2103=CARTESIAN_POINT('Ctrl Pts',(-40.3519323616533,232.002028447915,29.5533069226325));
#2104=CARTESIAN_POINT('Ctrl Pts',(-45.0327163383337,231.502028447915,23.1621886995185));
#2105=CARTESIAN_POINT('Ctrl Pts',(-47.5094422967239,231.002028447915,15.6374322712211));
#2106=CARTESIAN_POINT('Ctrl Pts',(-49.9861682551141,230.502028447915,8.11267584292358));
#2107=CARTESIAN_POINT('Ctrl Pts',(-50.0163970020424,230.002028447915,0.190856796705288));
#2108=CARTESIAN_POINT('Ctrl Pts',(-50.0466257489707,229.502028447915,-7.73096224951301));
#2109=CARTESIAN_POINT('Ctrl Pts',(-47.6273982840717,229.002028447915,-15.2744010708495));
#2110=CARTESIAN_POINT('Ctrl Pts',(-45.2081708191727,228.502028447915,-22.817839892186));
#2111=CARTESIAN_POINT('Ctrl Pts',(-40.5762979824596,228.002028447915,-29.2444941385794));
#2112=CARTESIAN_POINT('Ctrl Pts',(-35.9444251457465,227.502028447915,-35.6711483849729));
#2113=CARTESIAN_POINT('Ctrl Pts',(-29.5533069226325,227.002028447915,-40.3519323616533));
#2114=CARTESIAN_POINT('Ctrl Pts',(-23.1621886995185,226.502028447915,-45.0327163383337));
#2115=CARTESIAN_POINT('Ctrl Pts',(-15.6374322712211,226.002028447915,-47.5094422967239));
#2116=CARTESIAN_POINT('Ctrl Pts',(-8.11267584292359,225.502028447915,-49.9861682551141));
#2117=CARTESIAN_POINT('Ctrl Pts',(-0.190856796705292,225.002028447915,-50.0163970020424));
#2118=CARTESIAN_POINT('Ctrl Pts',(7.730962249513,224.502028447915,-50.0466257489707));
#2119=CARTESIAN_POINT('Ctrl Pts',(15.2744010708495,224.002028447915,-47.6273982840717));
#2120=CARTESIAN_POINT('Ctrl Pts',(22.817839892186,223.502028447915,-45.2081708191727));
#2121=CARTESIAN_POINT('Ctrl Pts',(29.2444941385794,223.002028447915,-40.5762979824596));
#2122=CARTESIAN_POINT('Ctrl Pts',(35.6711483849729,222.502028447915,-35.9444251457465));
#2123=CARTESIAN_POINT('Ctrl Pts',(40.3519323616533,222.002028447915,-29.5533069226325));
#2124=CARTESIAN_POINT('Ctrl Pts',(45.0327163383337,221.502028447915,-23.1621886995185));
#2125=CARTESIAN_POINT('Ctrl Pts',(47.5094422967239,221.002028447915,-15.6374322712211));
#2126=CARTESIAN_POINT('Ctrl Pts',(49.9861682551141,220.502028447915,-8.11267584292359));
#2127=CARTESIAN_POINT('Ctrl Pts',(50.0163970020424,220.002028447915,-0.190856796705295));
#2128=CARTESIAN_POINT('Ctrl Pts',(50.0466257489707,219.502028447915,7.730962249513));
#2129=CARTESIAN_POINT('Ctrl Pts',(47.6273982840717,219.002028447915,15.2744010708495));
#2130=CARTESIAN_POINT('Ctrl Pts',(45.2081708191727,218.502028447915,22.817839892186));
#2131=CARTESIAN_POINT('Ctrl Pts',(40.5762979824596,218.002028447915,29.2444941385794));
#2132=CARTESIAN_POINT('Ctrl Pts',(35.9444251457465,217.502028447915,35.6711483849729));
#2133=CARTESIAN_POINT('Ctrl Pts',(29.5533069226325,217.002028447915,40.3519323616533));
#2134=CARTESIAN_POINT('Ctrl Pts',(23.1621886995185,216.502028447915,45.0327163383337));
#2135=CARTESIAN_POINT('Ctrl Pts',(15.6374322712211,216.002028447915,47.5094422967239));
#2136=CARTESIAN_POINT('Ctrl Pts',(8.11267584292359,215.502028447915,49.9861682551141));
#2137=CARTESIAN_POINT('Ctrl Pts',(0.190856796705285,215.002028447915,50.0163970020424));
#2138=CARTESIAN_POINT('Ctrl Pts',(-7.73096224951301,214.502028447915,50.0466257489707));
#2139=CARTESIAN_POINT('Ctrl Pts',(-15.2744010708495,214.002028447915,47.6273982840717));
#2140=CARTESIAN_POINT('Ctrl Pts',(-22.817839892186,213.502028447915,45.2081708191727));
#2141=CARTESIAN_POINT('Ctrl Pts',(-29.2444941385794,213.002028447915,40.5762979824596));
#2142=CARTESIAN_POINT('Ctrl Pts',(-35.6711483849729,212.502028447915,35.9444251457465));
#2143=CARTESIAN_POINT('Ctrl Pts',(-40.3519323616533,212.002028447915,29.5533069226325));
#2144=CARTESIAN_POINT('Ctrl Pts',(-45.0327163383337,211.502028447915,23.1621886995185));
#2145=CARTESIAN_POINT('Ctrl Pts',(-47.5094422967239,211.002028447915,15.6374322712211));
#2146=CARTESIAN_POINT('Ctrl Pts',(-49.9861682551141,210.502028447915,8.11267584292358));
#2147=CARTESIAN_POINT('Ctrl Pts',(-50.0163970020424,210.002028447915,0.190856796705288));
#2148=CARTESIAN_POINT('Ctrl Pts',(-50.0466257489707,209.502028447915,-7.73096224951301));
#2149=CARTESIAN_POINT('Ctrl Pts',(-47.6273982840717,209.002028447915,-15.2744010708495));
#2150=CARTESIAN_POINT('Ctrl Pts',(-45.2081708191727,208.502028447915,-22.817839892186));
#2151=CARTESIAN_POINT('Ctrl Pts',(-40.5762979824596,208.002028447915,-29.2444941385794));
#2152=CARTESIAN_POINT('Ctrl Pts',(-35.9444251457465,207.502028447915,-35.6711483849729));
#2153=CARTESIAN_POINT('Ctrl Pts',(-29.5533069226325,207.002028447915,-40.3519323616533));
#2154=CARTESIAN_POINT('Ctrl Pts',(-23.1621886995185,206.502028447915,-45.0327163383337));
#2155=CARTESIAN_POINT('Ctrl Pts',(-15.6374322712211,206.002028447915,-47.5094422967239));
#2156=CARTESIAN_POINT('Ctrl Pts',(-8.11267584292359,205.502028447915,-49.9861682551141));
#2157=CARTESIAN_POINT('Ctrl Pts',(-0.190856796705292,205.002028447915,-50.0163970020424));
#2158=CARTESIAN_POINT('Ctrl Pts',(7.730962249513,204.502028447915,-50.0466257489707));
#2159=CARTESIAN_POINT('Ctrl Pts',(15.2744010708495,204.002028447915,-47.6273982840717));
#2160=CARTESIAN_POINT('Ctrl Pts',(22.817839892186,203.502028447915,-45.2081708191727));
#2161=CARTESIAN_POINT('Ctrl Pts',(29.2444941385794,203.002028447915,-40.5762979824596));
#2162=CARTESIAN_POINT('Ctrl Pts',(35.6711483849729,202.502028447915,-35.9444251457465));
#2163=CARTESIAN_POINT('Ctrl Pts',(40.3519323616533,202.002028447915,-29.5533069226325));
#2164=CARTESIAN_POINT('Ctrl Pts',(45.0327163383337,201.502028447915,-23.1621886995185));
#2165=CARTESIAN_POINT('Ctrl Pts',(47.5094422967239,201.002028447915,-15.6374322712211));
#2166=CARTESIAN_POINT('Ctrl Pts',(49.9861682551141,200.502028447915,-8.11267584292359));
#2167=CARTESIAN_POINT('Ctrl Pts',(50.0163970020424,200.002028447915,-0.190856796705295));
#2168=CARTESIAN_POINT('Ctrl Pts',(50.0466257489707,199.502028447915,7.730962249513));
#2169=CARTESIAN_POINT('Ctrl Pts',(47.6273982840717,199.002028447915,15.2744010708495));
#2170=CARTESIAN_POINT('Ctrl Pts',(45.2081708191727,198.502028447915,22.817839892186));
#2171=CARTESIAN_POINT('Ctrl Pts',(40.5762979824596,198.002028447915,29.2444941385794));
#2172=CARTESIAN_POINT('Ctrl Pts',(35.9444251457465,197.502028447915,35.6711483849729));
#2173=CARTESIAN_POINT('Ctrl Pts',(29.5533069226325,197.002028447915,40.3519323616533));
#2174=CARTESIAN_POINT('Ctrl Pts',(23.1621886995185,196.502028447915,45.0327163383337));
#2175=CARTESIAN_POINT('Ctrl Pts',(15.6374322712211,196.002028447915,47.5094422967239));
#2176=CARTESIAN_POINT('Ctrl Pts',(8.11267584292359,195.502028447915,49.9861682551141));
#2177=CARTESIAN_POINT('Ctrl Pts',(0.190856796705285,195.002028447915,50.0163970020424));
#2178=CARTESIAN_POINT('Ctrl Pts',(-7.73096224951301,194.502028447915,50.0466257489707));
#2179=CARTESIAN_POINT('Ctrl Pts',(-15.2744010708495,194.002028447915,47.6273982840717));
#2180=CARTESIAN_POINT('Ctrl Pts',(-22.817839892186,193.502028447915,45.2081708191727));
#2181=CARTESIAN_POINT('Ctrl Pts',(-29.2444941385794,193.002028447915,40.5762979824596));
#2182=CARTESIAN_POINT('Ctrl Pts',(-35.6711483849729,192.502028447915,35.9444251457465));
#2183=CARTESIAN_POINT('Ctrl Pts',(-40.3519323616533,192.002028447915,29.5533069226325));
#2184=CARTESIAN_POINT('Ctrl Pts',(-45.0327163383337,191.502028447915,23.1621886995185));
#2185=CARTESIAN_POINT('Ctrl Pts',(-47.5094422967239,191.002028447915,15.6374322712211));
#2186=CARTESIAN_POINT('Ctrl Pts',(-49.9861682551141,190.502028447915,8.11267584292358));
#2187=CARTESIAN_POINT('Ctrl Pts',(-50.0163970020424,190.002028447915,0.190856796705288));
#2188=CARTESIAN_POINT('Ctrl Pts',(-50.0466257489707,189.502028447915,-7.73096224951301));
#2189=CARTESIAN_POINT('Ctrl Pts',(-47.6273982840717,189.002028447915,-15.2744010708495));
#2190=CARTESIAN_POINT('Ctrl Pts',(-45.2081708191727,188.502028447915,-22.817839892186));
#2191=CARTESIAN_POINT('Ctrl Pts',(-40.5762979824596,188.002028447915,-29.2444941385794));
#2192=CARTESIAN_POINT('Ctrl Pts',(-35.9444251457465,187.502028447915,-35.6711483849729));
#2193=CARTESIAN_POINT('Ctrl Pts',(-29.5533069226325,187.002028447915,-40.3519323616533));
#2194=CARTESIAN_POINT('Ctrl Pts',(-23.1621886995185,186.502028447915,-45.0327163383337));
#2195=CARTESIAN_POINT('Ctrl Pts',(-15.6374322712211,186.002028447915,-47.5094422967239));
#2196=CARTESIAN_POINT('Ctrl Pts',(-8.11267584292359,185.502028447915,-49.9861682551141));
#2197=CARTESIAN_POINT('Ctrl Pts',(-0.190856796705292,185.002028447915,-50.0163970020424));
#2198=CARTESIAN_POINT('Ctrl Pts',(7.730962249513,184.502028447915,-50.0466257489707));
#2199=CARTESIAN_POINT('Ctrl Pts',(15.2744010708495,184.002028447915,-47.6273982840717));
#2200=CARTESIAN_POINT('Ctrl Pts',(22.817839892186,183.502028447915,-45.2081708191727));
#2201=CARTESIAN_POINT('Ctrl Pts',(29.2444941385794,183.002028447915,-40.5762979824596));
#2202=CARTESIAN_POINT('Ctrl Pts',(35.6711483849729,182.502028447915,-35.9444251457465));
#2203=CARTESIAN_POINT('Ctrl Pts',(40.3519323616533,182.002028447915,-29.5533069226325));
#2204=CARTESIAN_POINT('Ctrl Pts',(45.0327163383337,181.502028447915,-23.1621886995185));
#2205=CARTESIAN_POINT('Ctrl Pts',(47.5094422967239,181.002028447915,-15.6374322712211));
#2206=CARTESIAN_POINT('Ctrl Pts',(49.9861682551141,180.502028447915,-8.11267584292359));
#2207=CARTESIAN_POINT('Ctrl Pts',(50.0163970020424,180.002028447915,-0.190856796705295));
#2208=CARTESIAN_POINT('Ctrl Pts',(50.0466257489707,179.502028447915,7.730962249513));
#2209=CARTESIAN_POINT('Ctrl Pts',(47.6273982840717,179.002028447915,15.2744010708495));
#2210=CARTESIAN_POINT('Ctrl Pts',(45.2081708191727,178.502028447915,22.817839892186));
#2211=CARTESIAN_POINT('Ctrl Pts',(40.5762979824596,178.002028447915,29.2444941385794));
#2212=CARTESIAN_POINT('Ctrl Pts',(35.9444251457465,177.502028447915,35.6711483849729));
#2213=CARTESIAN_POINT('Ctrl Pts',(29.5533069226325,177.002028447915,40.3519323616533));
#2214=CARTESIAN_POINT('Ctrl Pts',(23.1621886995185,176.502028447915,45.0327163383337));
#2215=CARTESIAN_POINT('Ctrl Pts',(15.6374322712211,176.002028447915,47.5094422967239));
#2216=CARTESIAN_POINT('Ctrl Pts',(8.11267584292359,175.502028447915,49.9861682551141));
#2217=CARTESIAN_POINT('Ctrl Pts',(0.190856796705285,175.002028447915,50.0163970020424));
#2218=CARTESIAN_POINT('Ctrl Pts',(0.000256710972400879,237.995967593475,
50.0163970020424));
#2219=CARTESIAN_POINT('Ctrl Pts',(-7.92156233524589,237.495967593475,50.0164376610661));
#2220=CARTESIAN_POINT('Ctrl Pts',(-15.4556725243922,236.995967593475,47.5684996184509));
#2221=CARTESIAN_POINT('Ctrl Pts',(-22.9897827135384,236.495967593475,45.1205615758357));
#2222=CARTESIAN_POINT('Ctrl Pts',(-29.3986928470667,235.995967593475,40.4642660629801));
#2223=CARTESIAN_POINT('Ctrl Pts',(-35.8076029805949,235.495967593475,35.8079705501245));
#2224=CARTESIAN_POINT('Ctrl Pts',(-40.4639642811328,234.995967593475,29.3991082141453));
#2225=CARTESIAN_POINT('Ctrl Pts',(-45.1203255816707,234.495967593475,22.990245878166));
#2226=CARTESIAN_POINT('Ctrl Pts',(-47.5683409623447,233.995967593475,15.4561608176784));
#2227=CARTESIAN_POINT('Ctrl Pts',(-50.0163563430187,233.495967593475,7.9220757571907));
#2228=CARTESIAN_POINT('Ctrl Pts',(-50.0163970020424,232.995967593475,0.000256710972403942));
#2229=CARTESIAN_POINT('Ctrl Pts',(-50.0164376610661,232.495967593475,-7.92156233524589));
#2230=CARTESIAN_POINT('Ctrl Pts',(-47.5684996184509,231.995967593475,-15.4556725243922));
#2231=CARTESIAN_POINT('Ctrl Pts',(-45.1205615758357,231.495967593475,-22.9897827135384));
#2232=CARTESIAN_POINT('Ctrl Pts',(-40.4642660629801,230.995967593475,-29.3986928470667));
#2233=CARTESIAN_POINT('Ctrl Pts',(-35.8079705501245,230.495967593475,-35.8076029805949));
#2234=CARTESIAN_POINT('Ctrl Pts',(-29.3991082141453,229.995967593475,-40.4639642811328));
#2235=CARTESIAN_POINT('Ctrl Pts',(-22.9902458781661,229.495967593475,-45.1203255816707));
#2236=CARTESIAN_POINT('Ctrl Pts',(-15.4561608176784,228.995967593475,-47.5683409623447));
#2237=CARTESIAN_POINT('Ctrl Pts',(-7.92207575719071,228.495967593475,-50.0163563430187));
#2238=CARTESIAN_POINT('Ctrl Pts',(-0.000256710972407005,227.995967593475,
-50.0163970020424));
#2239=CARTESIAN_POINT('Ctrl Pts',(7.92156233524589,227.495967593475,-50.0164376610661));
#2240=CARTESIAN_POINT('Ctrl Pts',(15.4556725243922,226.995967593475,-47.5684996184509));
#2241=CARTESIAN_POINT('Ctrl Pts',(22.9897827135384,226.495967593475,-45.1205615758357));
#2242=CARTESIAN_POINT('Ctrl Pts',(29.3986928470667,225.995967593475,-40.4642660629801));
#2243=CARTESIAN_POINT('Ctrl Pts',(35.8076029805949,225.495967593475,-35.8079705501245));
#2244=CARTESIAN_POINT('Ctrl Pts',(40.4639642811328,224.995967593475,-29.3991082141453));
#2245=CARTESIAN_POINT('Ctrl Pts',(45.1203255816707,224.495967593475,-22.9902458781661));
#2246=CARTESIAN_POINT('Ctrl Pts',(47.5683409623447,223.995967593475,-15.4561608176784));
#2247=CARTESIAN_POINT('Ctrl Pts',(50.0163563430187,223.495967593475,-7.92207575719071));
#2248=CARTESIAN_POINT('Ctrl Pts',(50.0163970020424,222.995967593475,-0.000256710972410067));
#2249=CARTESIAN_POINT('Ctrl Pts',(50.0164376610661,222.495967593475,7.92156233524589));
#2250=CARTESIAN_POINT('Ctrl Pts',(47.5684996184509,221.995967593475,15.4556725243922));
#2251=CARTESIAN_POINT('Ctrl Pts',(45.1205615758358,221.495967593475,22.9897827135384));
#2252=CARTESIAN_POINT('Ctrl Pts',(40.4642660629801,220.995967593475,29.3986928470667));
#2253=CARTESIAN_POINT('Ctrl Pts',(35.8079705501245,220.495967593475,35.8076029805949));
#2254=CARTESIAN_POINT('Ctrl Pts',(29.3991082141453,219.995967593475,40.4639642811328));
#2255=CARTESIAN_POINT('Ctrl Pts',(22.9902458781661,219.495967593475,45.1203255816707));
#2256=CARTESIAN_POINT('Ctrl Pts',(15.4561608176784,218.995967593475,47.5683409623447));
#2257=CARTESIAN_POINT('Ctrl Pts',(7.92207575719071,218.495967593475,50.0163563430187));
#2258=CARTESIAN_POINT('Ctrl Pts',(0.000256710972400879,217.995967593475,
50.0163970020424));
#2259=CARTESIAN_POINT('Ctrl Pts',(-7.92156233524589,217.495967593475,50.0164376610661));
#2260=CARTESIAN_POINT('Ctrl Pts',(-15.4556725243922,216.995967593475,47.5684996184509));
#2261=CARTESIAN_POINT('Ctrl Pts',(-22.9897827135384,216.495967593475,45.1205615758357));
#2262=CARTESIAN_POINT('Ctrl Pts',(-29.3986928470667,215.995967593475,40.4642660629801));
#2263=CARTESIAN_POINT('Ctrl Pts',(-35.8076029805949,215.495967593475,35.8079705501245));
#2264=CARTESIAN_POINT('Ctrl Pts',(-40.4639642811328,214.995967593475,29.3991082141453));
#2265=CARTESIAN_POINT('Ctrl Pts',(-45.1203255816707,214.495967593475,22.990245878166));
#2266=CARTESIAN_POINT('Ctrl Pts',(-47.5683409623447,213.995967593475,15.4561608176784));
#2267=CARTESIAN_POINT('Ctrl Pts',(-50.0163563430187,213.495967593475,7.9220757571907));
#2268=CARTESIAN_POINT('Ctrl Pts',(-50.0163970020424,212.995967593475,0.000256710972403942));
#2269=CARTESIAN_POINT('Ctrl Pts',(-50.0164376610661,212.495967593475,-7.92156233524589));
#2270=CARTESIAN_POINT('Ctrl Pts',(-47.5684996184509,211.995967593475,-15.4556725243922));
#2271=CARTESIAN_POINT('Ctrl Pts',(-45.1205615758357,211.495967593475,-22.9897827135384));
#2272=CARTESIAN_POINT('Ctrl Pts',(-40.4642660629801,210.995967593475,-29.3986928470667));
#2273=CARTESIAN_POINT('Ctrl Pts',(-35.8079705501245,210.495967593475,-35.8076029805949));
#2274=CARTESIAN_POINT('Ctrl Pts',(-29.3991082141453,209.995967593475,-40.4639642811328));
#2275=CARTESIAN_POINT('Ctrl Pts',(-22.9902458781661,209.495967593475,-45.1203255816707));
#2276=CARTESIAN_POINT('Ctrl Pts',(-15.4561608176784,208.995967593475,-47.5683409623447));
#2277=CARTESIAN_POINT('Ctrl Pts',(-7.92207575719071,208.495967593475,-50.0163563430187));
#2278=CARTESIAN_POINT('Ctrl Pts',(-0.000256710972407005,207.995967593475,
-50.0163970020424));
#2279=CARTESIAN_POINT('Ctrl Pts',(7.92156233524589,207.495967593475,-50.0164376610661));
#2280=CARTESIAN_POINT('Ctrl Pts',(15.4556725243922,206.995967593475,-47.5684996184509));
#2281=CARTESIAN_POINT('Ctrl Pts',(22.9897827135384,206.495967593475,-45.1205615758357));
#2282=CARTESIAN_POINT('Ctrl Pts',(29.3986928470667,205.995967593475,-40.4642660629801));
#2283=CARTESIAN_POINT('Ctrl Pts',(35.8076029805949,205.495967593475,-35.8079705501245));
#2284=CARTESIAN_POINT('Ctrl Pts',(40.4639642811328,204.995967593475,-29.3991082141453));
#2285=CARTESIAN_POINT('Ctrl Pts',(45.1203255816707,204.495967593475,-22.9902458781661));
#2286=CARTESIAN_POINT('Ctrl Pts',(47.5683409623447,203.995967593475,-15.4561608176784));
#2287=CARTESIAN_POINT('Ctrl Pts',(50.0163563430187,203.495967593475,-7.92207575719071));
#2288=CARTESIAN_POINT('Ctrl Pts',(50.0163970020424,202.995967593475,-0.000256710972410067));
#2289=CARTESIAN_POINT('Ctrl Pts',(50.0164376610661,202.495967593475,7.92156233524589));
#2290=CARTESIAN_POINT('Ctrl Pts',(47.5684996184509,201.995967593475,15.4556725243922));
#2291=CARTESIAN_POINT('Ctrl Pts',(45.1205615758358,201.495967593475,22.9897827135384));
#2292=CARTESIAN_POINT('Ctrl Pts',(40.4642660629801,200.995967593475,29.3986928470667));
#2293=CARTESIAN_POINT('Ctrl Pts',(35.8079705501245,200.495967593475,35.8076029805949));
#2294=CARTESIAN_POINT('Ctrl Pts',(29.3991082141453,199.995967593475,40.4639642811328));
#2295=CARTESIAN_POINT('Ctrl Pts',(22.9902458781661,199.495967593475,45.1203255816707));
#2296=CARTESIAN_POINT('Ctrl Pts',(15.4561608176784,198.995967593475,47.5683409623447));
#2297=CARTESIAN_POINT('Ctrl Pts',(7.92207575719071,198.495967593475,50.0163563430187));
#2298=CARTESIAN_POINT('Ctrl Pts',(0.000256710972400879,197.995967593475,
50.0163970020424));
#2299=CARTESIAN_POINT('Ctrl Pts',(-7.92156233524589,197.495967593475,50.0164376610661));
#2300=CARTESIAN_POINT('Ctrl Pts',(-15.4556725243922,196.995967593475,47.5684996184509));
#2301=CARTESIAN_POINT('Ctrl Pts',(-22.9897827135384,196.495967593475,45.1205615758357));
#2302=CARTESIAN_POINT('Ctrl Pts',(-29.3986928470667,195.995967593475,40.4642660629801));
#2303=CARTESIAN_POINT('Ctrl Pts',(-35.8076029805949,195.495967593475,35.8079705501245));
#2304=CARTESIAN_POINT('Ctrl Pts',(-40.4639642811328,194.995967593475,29.3991082141453));
#2305=CARTESIAN_POINT('Ctrl Pts',(-45.1203255816707,194.495967593475,22.990245878166));
#2306=CARTESIAN_POINT('Ctrl Pts',(-47.5683409623447,193.995967593475,15.4561608176784));
#2307=CARTESIAN_POINT('Ctrl Pts',(-50.0163563430187,193.495967593475,7.9220757571907));
#2308=CARTESIAN_POINT('Ctrl Pts',(-50.0163970020424,192.995967593475,0.000256710972403942));
#2309=CARTESIAN_POINT('Ctrl Pts',(-50.0164376610661,192.495967593475,-7.92156233524589));
#2310=CARTESIAN_POINT('Ctrl Pts',(-47.5684996184509,191.995967593475,-15.4556725243922));
#2311=CARTESIAN_POINT('Ctrl Pts',(-45.1205615758357,191.495967593475,-22.9897827135384));
#2312=CARTESIAN_POINT('Ctrl Pts',(-40.4642660629801,190.995967593475,-29.3986928470667));
#2313=CARTESIAN_POINT('Ctrl Pts',(-35.8079705501245,190.495967593475,-35.8076029805949));
#2314=CARTESIAN_POINT('Ctrl Pts',(-29.3991082141453,189.995967593475,-40.4639642811328));
#2315=CARTESIAN_POINT('Ctrl Pts',(-22.9902458781661,189.495967593475,-45.1203255816707));
#2316=CARTESIAN_POINT('Ctrl Pts',(-15.4561608176784,188.995967593475,-47.5683409623447));
#2317=CARTESIAN_POINT('Ctrl Pts',(-7.92207575719071,188.495967593475,-50.0163563430187));
#2318=CARTESIAN_POINT('Ctrl Pts',(-0.000256710972407005,187.995967593475,
-50.0163970020424));
#2319=CARTESIAN_POINT('Ctrl Pts',(7.92156233524589,187.495967593475,-50.0164376610661));
#2320=CARTESIAN_POINT('Ctrl Pts',(15.4556725243922,186.995967593475,-47.5684996184509));
#2321=CARTESIAN_POINT('Ctrl Pts',(22.9897827135384,186.495967593475,-45.1205615758357));
#2322=CARTESIAN_POINT('Ctrl Pts',(29.3986928470667,185.995967593475,-40.4642660629801));
#2323=CARTESIAN_POINT('Ctrl Pts',(35.8076029805949,185.495967593475,-35.8079705501245));
#2324=CARTESIAN_POINT('Ctrl Pts',(40.4639642811328,184.995967593475,-29.3991082141453));
#2325=CARTESIAN_POINT('Ctrl Pts',(45.1203255816707,184.495967593475,-22.9902458781661));
#2326=CARTESIAN_POINT('Ctrl Pts',(47.5683409623447,183.995967593475,-15.4561608176784));
#2327=CARTESIAN_POINT('Ctrl Pts',(50.0163563430187,183.495967593475,-7.92207575719071));
#2328=CARTESIAN_POINT('Ctrl Pts',(50.0163970020424,182.995967593475,-0.000256710972410067));
#2329=CARTESIAN_POINT('Ctrl Pts',(50.0164376610661,182.495967593475,7.92156233524589));
#2330=CARTESIAN_POINT('Ctrl Pts',(47.5684996184509,181.995967593475,15.4556725243922));
#2331=CARTESIAN_POINT('Ctrl Pts',(45.1205615758358,181.495967593475,22.9897827135384));
#2332=CARTESIAN_POINT('Ctrl Pts',(40.4642660629801,180.995967593475,29.3986928470667));
#2333=CARTESIAN_POINT('Ctrl Pts',(35.8079705501245,180.495967593475,35.8076029805949));
#2334=CARTESIAN_POINT('Ctrl Pts',(29.3991082141453,179.995967593475,40.4639642811328));
#2335=CARTESIAN_POINT('Ctrl Pts',(22.9902458781661,179.495967593475,45.1203255816707));
#2336=CARTESIAN_POINT('Ctrl Pts',(15.4561608176784,178.995967593475,47.5683409623447));
#2337=CARTESIAN_POINT('Ctrl Pts',(7.92207575719071,178.495967593475,50.0163563430187));
#2338=CARTESIAN_POINT('Ctrl Pts',(0.000256710972400879,177.995967593475,
50.0163970020424));
#2339=CARTESIAN_POINT('Ctrl Pts',(0.00025671097240121,237.995967593475,
7.5));
#2340=CARTESIAN_POINT('Ctrl Pts',(-1.18762659146162,237.495967593475,7.50004065902369));
#2341=CARTESIAN_POINT('Ctrl Pts',(-2.317383311169,236.995967593475,7.13300320026677));
#2342=CARTESIAN_POINT('Ctrl Pts',(-3.44714003087638,236.495967593475,6.76596574150984));
#2343=CARTESIAN_POINT('Ctrl Pts',(-4.40818170865423,235.995967593475,6.06777834873578));
#2344=CARTESIAN_POINT('Ctrl Pts',(-5.36922338643209,235.495967593475,5.36959095596173));
#2345=CARTESIAN_POINT('Ctrl Pts',(-6.06747656688843,234.995967593475,4.40859707573286));
#2346=CARTESIAN_POINT('Ctrl Pts',(-6.76572974734476,234.495967593475,3.447603195504));
#2347=CARTESIAN_POINT('Ctrl Pts',(-7.13284454416054,233.995967593475,2.31787160445521));
#2348=CARTESIAN_POINT('Ctrl Pts',(-7.49995934097631,233.495967593475,1.18814001340642));
#2349=CARTESIAN_POINT('Ctrl Pts',(-7.5,232.995967593475,0.000256710972401669));
#2350=CARTESIAN_POINT('Ctrl Pts',(-7.50004065902369,232.495967593475,-1.18762659146162));
#2351=CARTESIAN_POINT('Ctrl Pts',(-7.13300320026677,231.995967593475,-2.317383311169));
#2352=CARTESIAN_POINT('Ctrl Pts',(-6.76596574150984,231.495967593475,-3.44714003087638));
#2353=CARTESIAN_POINT('Ctrl Pts',(-6.06777834873578,230.995967593475,-4.40818170865423));
#2354=CARTESIAN_POINT('Ctrl Pts',(-5.36959095596173,230.495967593475,-5.36922338643209));
#2355=CARTESIAN_POINT('Ctrl Pts',(-4.40859707573286,229.995967593475,-6.06747656688843));
#2356=CARTESIAN_POINT('Ctrl Pts',(-3.447603195504,229.495967593475,-6.76572974734476));
#2357=CARTESIAN_POINT('Ctrl Pts',(-2.31787160445521,228.995967593475,-7.13284454416054));
#2358=CARTESIAN_POINT('Ctrl Pts',(-1.18814001340642,228.495967593475,-7.49995934097631));
#2359=CARTESIAN_POINT('Ctrl Pts',(-0.000256710972402128,227.995967593475,
-7.5));
#2360=CARTESIAN_POINT('Ctrl Pts',(1.18762659146162,227.495967593475,-7.50004065902369));
#2361=CARTESIAN_POINT('Ctrl Pts',(2.317383311169,226.995967593475,-7.13300320026677));
#2362=CARTESIAN_POINT('Ctrl Pts',(3.44714003087638,226.495967593475,-6.76596574150984));
#2363=CARTESIAN_POINT('Ctrl Pts',(4.40818170865423,225.995967593475,-6.06777834873578));
#2364=CARTESIAN_POINT('Ctrl Pts',(5.36922338643209,225.495967593475,-5.36959095596173));
#2365=CARTESIAN_POINT('Ctrl Pts',(6.06747656688843,224.995967593475,-4.40859707573286));
#2366=CARTESIAN_POINT('Ctrl Pts',(6.76572974734476,224.495967593475,-3.447603195504));
#2367=CARTESIAN_POINT('Ctrl Pts',(7.13284454416054,223.995967593475,-2.31787160445521));
#2368=CARTESIAN_POINT('Ctrl Pts',(7.49995934097631,223.495967593475,-1.18814001340642));
#2369=CARTESIAN_POINT('Ctrl Pts',(7.5,222.995967593475,-0.000256710972402588));
#2370=CARTESIAN_POINT('Ctrl Pts',(7.50004065902369,222.495967593475,1.18762659146162));
#2371=CARTESIAN_POINT('Ctrl Pts',(7.13300320026677,221.995967593475,2.317383311169));
#2372=CARTESIAN_POINT('Ctrl Pts',(6.76596574150984,221.495967593475,3.44714003087638));
#2373=CARTESIAN_POINT('Ctrl Pts',(6.06777834873579,220.995967593475,4.40818170865423));
#2374=CARTESIAN_POINT('Ctrl Pts',(5.36959095596173,220.495967593475,5.36922338643209));
#2375=CARTESIAN_POINT('Ctrl Pts',(4.40859707573286,219.995967593475,6.06747656688843));
#2376=CARTESIAN_POINT('Ctrl Pts',(3.447603195504,219.495967593475,6.76572974734476));
#2377=CARTESIAN_POINT('Ctrl Pts',(2.31787160445521,218.995967593475,7.13284454416054));
#2378=CARTESIAN_POINT('Ctrl Pts',(1.18814001340643,218.495967593475,7.49995934097631));
#2379=CARTESIAN_POINT('Ctrl Pts',(0.00025671097240121,217.995967593475,
7.5));
#2380=CARTESIAN_POINT('Ctrl Pts',(-1.18762659146162,217.495967593475,7.50004065902369));
#2381=CARTESIAN_POINT('Ctrl Pts',(-2.317383311169,216.995967593475,7.13300320026677));
#2382=CARTESIAN_POINT('Ctrl Pts',(-3.44714003087638,216.495967593475,6.76596574150984));
#2383=CARTESIAN_POINT('Ctrl Pts',(-4.40818170865423,215.995967593475,6.06777834873578));
#2384=CARTESIAN_POINT('Ctrl Pts',(-5.36922338643209,215.495967593475,5.36959095596173));
#2385=CARTESIAN_POINT('Ctrl Pts',(-6.06747656688843,214.995967593475,4.40859707573286));
#2386=CARTESIAN_POINT('Ctrl Pts',(-6.76572974734476,214.495967593475,3.447603195504));
#2387=CARTESIAN_POINT('Ctrl Pts',(-7.13284454416054,213.995967593475,2.31787160445521));
#2388=CARTESIAN_POINT('Ctrl Pts',(-7.49995934097631,213.495967593475,1.18814001340642));
#2389=CARTESIAN_POINT('Ctrl Pts',(-7.5,212.995967593475,0.000256710972401669));
#2390=CARTESIAN_POINT('Ctrl Pts',(-7.50004065902369,212.495967593475,-1.18762659146162));
#2391=CARTESIAN_POINT('Ctrl Pts',(-7.13300320026677,211.995967593475,-2.317383311169));
#2392=CARTESIAN_POINT('Ctrl Pts',(-6.76596574150984,211.495967593475,-3.44714003087638));
#2393=CARTESIAN_POINT('Ctrl Pts',(-6.06777834873578,210.995967593475,-4.40818170865423));
#2394=CARTESIAN_POINT('Ctrl Pts',(-5.36959095596173,210.495967593475,-5.36922338643209));
#2395=CARTESIAN_POINT('Ctrl Pts',(-4.40859707573286,209.995967593475,-6.06747656688843));
#2396=CARTESIAN_POINT('Ctrl Pts',(-3.447603195504,209.495967593475,-6.76572974734476));
#2397=CARTESIAN_POINT('Ctrl Pts',(-2.31787160445521,208.995967593475,-7.13284454416054));
#2398=CARTESIAN_POINT('Ctrl Pts',(-1.18814001340642,208.495967593475,-7.49995934097631));
#2399=CARTESIAN_POINT('Ctrl Pts',(-0.000256710972402128,207.995967593475,
-7.5));
#2400=CARTESIAN_POINT('Ctrl Pts',(1.18762659146162,207.495967593475,-7.50004065902369));
#2401=CARTESIAN_POINT('Ctrl Pts',(2.317383311169,206.995967593475,-7.13300320026677));
#2402=CARTESIAN_POINT('Ctrl Pts',(3.44714003087638,206.495967593475,-6.76596574150984));
#2403=CARTESIAN_POINT('Ctrl Pts',(4.40818170865423,205.995967593475,-6.06777834873578));
#2404=CARTESIAN_POINT('Ctrl Pts',(5.36922338643209,205.495967593475,-5.36959095596173));
#2405=CARTESIAN_POINT('Ctrl Pts',(6.06747656688843,204.995967593475,-4.40859707573286));
#2406=CARTESIAN_POINT('Ctrl Pts',(6.76572974734476,204.495967593475,-3.447603195504));
#2407=CARTESIAN_POINT('Ctrl Pts',(7.13284454416054,203.995967593475,-2.31787160445521));
#2408=CARTESIAN_POINT('Ctrl Pts',(7.49995934097631,203.495967593475,-1.18814001340642));
#2409=CARTESIAN_POINT('Ctrl Pts',(7.5,202.995967593475,-0.000256710972402588));
#2410=CARTESIAN_POINT('Ctrl Pts',(7.50004065902369,202.495967593475,1.18762659146162));
#2411=CARTESIAN_POINT('Ctrl Pts',(7.13300320026677,201.995967593475,2.317383311169));
#2412=CARTESIAN_POINT('Ctrl Pts',(6.76596574150984,201.495967593475,3.44714003087638));
#2413=CARTESIAN_POINT('Ctrl Pts',(6.06777834873579,200.995967593475,4.40818170865423));
#2414=CARTESIAN_POINT('Ctrl Pts',(5.36959095596173,200.495967593475,5.36922338643209));
#2415=CARTESIAN_POINT('Ctrl Pts',(4.40859707573286,199.995967593475,6.06747656688843));
#2416=CARTESIAN_POINT('Ctrl Pts',(3.447603195504,199.495967593475,6.76572974734476));
#2417=CARTESIAN_POINT('Ctrl Pts',(2.31787160445521,198.995967593475,7.13284454416054));
#2418=CARTESIAN_POINT('Ctrl Pts',(1.18814001340643,198.495967593475,7.49995934097631));
#2419=CARTESIAN_POINT('Ctrl Pts',(0.00025671097240121,197.995967593475,
7.5));
#2420=CARTESIAN_POINT('Ctrl Pts',(-1.18762659146162,197.495967593475,7.50004065902369));
#2421=CARTESIAN_POINT('Ctrl Pts',(-2.317383311169,196.995967593475,7.13300320026677));
#2422=CARTESIAN_POINT('Ctrl Pts',(-3.44714003087638,196.495967593475,6.76596574150984));
#2423=CARTESIAN_POINT('Ctrl Pts',(-4.40818170865423,195.995967593475,6.06777834873578));
#2424=CARTESIAN_POINT('Ctrl Pts',(-5.36922338643209,195.495967593475,5.36959095596173));
#2425=CARTESIAN_POINT('Ctrl Pts',(-6.06747656688843,194.995967593475,4.40859707573286));
#2426=CARTESIAN_POINT('Ctrl Pts',(-6.76572974734476,194.495967593475,3.447603195504));
#2427=CARTESIAN_POINT('Ctrl Pts',(-7.13284454416054,193.995967593475,2.31787160445521));
#2428=CARTESIAN_POINT('Ctrl Pts',(-7.49995934097631,193.495967593475,1.18814001340642));
#2429=CARTESIAN_POINT('Ctrl Pts',(-7.5,192.995967593475,0.000256710972401669));
#2430=CARTESIAN_POINT('Ctrl Pts',(-7.50004065902369,192.495967593475,-1.18762659146162));
#2431=CARTESIAN_POINT('Ctrl Pts',(-7.13300320026677,191.995967593475,-2.317383311169));
#2432=CARTESIAN_POINT('Ctrl Pts',(-6.76596574150984,191.495967593475,-3.44714003087638));
#2433=CARTESIAN_POINT('Ctrl Pts',(-6.06777834873578,190.995967593475,-4.40818170865423));
#2434=CARTESIAN_POINT('Ctrl Pts',(-5.36959095596173,190.495967593475,-5.36922338643209));
#2435=CARTESIAN_POINT('Ctrl Pts',(-4.40859707573286,189.995967593475,-6.06747656688843));
#2436=CARTESIAN_POINT('Ctrl Pts',(-3.447603195504,189.495967593475,-6.76572974734476));
#2437=CARTESIAN_POINT('Ctrl Pts',(-2.31787160445521,188.995967593475,-7.13284454416054));
#2438=CARTESIAN_POINT('Ctrl Pts',(-1.18814001340642,188.495967593475,-7.49995934097631));
#2439=CARTESIAN_POINT('Ctrl Pts',(-0.000256710972402128,187.995967593475,
-7.5));
#2440=CARTESIAN_POINT('Ctrl Pts',(1.18762659146162,187.495967593475,-7.50004065902369));
#2441=CARTESIAN_POINT('Ctrl Pts',(2.317383311169,186.995967593475,-7.13300320026677));
#2442=CARTESIAN_POINT('Ctrl Pts',(3.44714003087638,186.495967593475,-6.76596574150984));
#2443=CARTESIAN_POINT('Ctrl Pts',(4.40818170865423,185.995967593475,-6.06777834873578));
#2444=CARTESIAN_POINT('Ctrl Pts',(5.36922338643209,185.495967593475,-5.36959095596173));
#2445=CARTESIAN_POINT('Ctrl Pts',(6.06747656688843,184.995967593475,-4.40859707573286));
#2446=CARTESIAN_POINT('Ctrl Pts',(6.76572974734476,184.495967593475,-3.447603195504));
#2447=CARTESIAN_POINT('Ctrl Pts',(7.13284454416054,183.995967593475,-2.31787160445521));
#2448=CARTESIAN_POINT('Ctrl Pts',(7.49995934097631,183.495967593475,-1.18814001340642));
#2449=CARTESIAN_POINT('Ctrl Pts',(7.5,182.995967593475,-0.000256710972402588));
#2450=CARTESIAN_POINT('Ctrl Pts',(7.50004065902369,182.495967593475,1.18762659146162));
#2451=CARTESIAN_POINT('Ctrl Pts',(7.13300320026677,181.995967593475,2.317383311169));
#2452=CARTESIAN_POINT('Ctrl Pts',(6.76596574150984,181.495967593475,3.44714003087638));
#2453=CARTESIAN_POINT('Ctrl Pts',(6.06777834873579,180.995967593475,4.40818170865423));
#2454=CARTESIAN_POINT('Ctrl Pts',(5.36959095596173,180.495967593475,5.36922338643209));
#2455=CARTESIAN_POINT('Ctrl Pts',(4.40859707573286,179.995967593475,6.06747656688843));
#2456=CARTESIAN_POINT('Ctrl Pts',(3.447603195504,179.495967593475,6.76572974734476));
#2457=CARTESIAN_POINT('Ctrl Pts',(2.31787160445521,178.995967593475,7.13284454416054));
#2458=CARTESIAN_POINT('Ctrl Pts',(1.18814001340643,178.495967593475,7.49995934097631));
#2459=CARTESIAN_POINT('Ctrl Pts',(0.00025671097240121,177.995967593475,
7.5));
#2460=CARTESIAN_POINT('Ctrl Pts',(0.000256710972400845,237.995967593475,
50.0163970020424));
#2461=CARTESIAN_POINT('Ctrl Pts',(-7.92156233524589,237.495967593475,50.0164376610661));
#2462=CARTESIAN_POINT('Ctrl Pts',(-15.4556725243922,236.995967593475,47.5684996184509));
#2463=CARTESIAN_POINT('Ctrl Pts',(-22.9897827135384,236.495967593475,45.1205615758357));
#2464=CARTESIAN_POINT('Ctrl Pts',(-29.3986928470667,235.995967593475,40.4642660629801));
#2465=CARTESIAN_POINT('Ctrl Pts',(-35.8076029805949,235.495967593475,35.8079705501245));
#2466=CARTESIAN_POINT('Ctrl Pts',(-40.4639642811328,234.995967593475,29.3991082141453));
#2467=CARTESIAN_POINT('Ctrl Pts',(-45.1203255816707,234.495967593475,22.990245878166));
#2468=CARTESIAN_POINT('Ctrl Pts',(-47.5683409623447,233.995967593475,15.4561608176784));
#2469=CARTESIAN_POINT('Ctrl Pts',(-50.0163563430187,233.495967593475,7.9220757571907));
#2470=CARTESIAN_POINT('Ctrl Pts',(-50.0163970020424,232.995967593475,0.000256710972403907));
#2471=CARTESIAN_POINT('Ctrl Pts',(-50.0164376610661,232.495967593475,-7.92156233524589));
#2472=CARTESIAN_POINT('Ctrl Pts',(-47.5684996184509,231.995967593475,-15.4556725243922));
#2473=CARTESIAN_POINT('Ctrl Pts',(-45.1205615758357,231.495967593475,-22.9897827135384));
#2474=CARTESIAN_POINT('Ctrl Pts',(-40.4642660629801,230.995967593475,-29.3986928470667));
#2475=CARTESIAN_POINT('Ctrl Pts',(-35.8079705501245,230.495967593475,-35.8076029805949));
#2476=CARTESIAN_POINT('Ctrl Pts',(-29.3991082141453,229.995967593475,-40.4639642811328));
#2477=CARTESIAN_POINT('Ctrl Pts',(-22.9902458781661,229.495967593475,-45.1203255816707));
#2478=CARTESIAN_POINT('Ctrl Pts',(-15.4561608176784,228.995967593475,-47.5683409623447));
#2479=CARTESIAN_POINT('Ctrl Pts',(-7.92207575719071,228.495967593475,-50.0163563430187));
#2480=CARTESIAN_POINT('Ctrl Pts',(-0.00025671097240697,227.995967593475,
-50.0163970020424));
#2481=CARTESIAN_POINT('Ctrl Pts',(7.92156233524589,227.495967593475,-50.0164376610661));
#2482=CARTESIAN_POINT('Ctrl Pts',(15.4556725243922,226.995967593475,-47.5684996184509));
#2483=CARTESIAN_POINT('Ctrl Pts',(22.9897827135384,226.495967593475,-45.1205615758357));
#2484=CARTESIAN_POINT('Ctrl Pts',(29.3986928470667,225.995967593475,-40.4642660629801));
#2485=CARTESIAN_POINT('Ctrl Pts',(35.8076029805949,225.495967593475,-35.8079705501245));
#2486=CARTESIAN_POINT('Ctrl Pts',(40.4639642811328,224.995967593475,-29.3991082141453));
#2487=CARTESIAN_POINT('Ctrl Pts',(45.1203255816707,224.495967593475,-22.9902458781661));
#2488=CARTESIAN_POINT('Ctrl Pts',(47.5683409623447,223.995967593475,-15.4561608176784));
#2489=CARTESIAN_POINT('Ctrl Pts',(50.0163563430187,223.495967593475,-7.92207575719071));
#2490=CARTESIAN_POINT('Ctrl Pts',(50.0163970020424,222.995967593475,-0.000256710972410033));
#2491=CARTESIAN_POINT('Ctrl Pts',(50.0164376610661,222.495967593475,7.92156233524589));
#2492=CARTESIAN_POINT('Ctrl Pts',(47.5684996184509,221.995967593475,15.4556725243922));
#2493=CARTESIAN_POINT('Ctrl Pts',(45.1205615758358,221.495967593475,22.9897827135384));
#2494=CARTESIAN_POINT('Ctrl Pts',(40.4642660629801,220.995967593475,29.3986928470667));
#2495=CARTESIAN_POINT('Ctrl Pts',(35.8079705501245,220.495967593475,35.8076029805949));
#2496=CARTESIAN_POINT('Ctrl Pts',(29.3991082141453,219.995967593475,40.4639642811328));
#2497=CARTESIAN_POINT('Ctrl Pts',(22.9902458781661,219.495967593475,45.1203255816707));
#2498=CARTESIAN_POINT('Ctrl Pts',(15.4561608176784,218.995967593475,47.5683409623447));
#2499=CARTESIAN_POINT('Ctrl Pts',(7.92207575719071,218.495967593475,50.0163563430187));
#2500=CARTESIAN_POINT('Ctrl Pts',(0.000256710972400845,217.995967593475,
50.0163970020424));
#2501=CARTESIAN_POINT('Ctrl Pts',(-7.92156233524589,217.495967593475,50.0164376610661));
#2502=CARTESIAN_POINT('Ctrl Pts',(-15.4556725243922,216.995967593475,47.5684996184509));
#2503=CARTESIAN_POINT('Ctrl Pts',(-22.9897827135384,216.495967593475,45.1205615758357));
#2504=CARTESIAN_POINT('Ctrl Pts',(-29.3986928470667,215.995967593475,40.4642660629801));
#2505=CARTESIAN_POINT('Ctrl Pts',(-35.8076029805949,215.495967593475,35.8079705501245));
#2506=CARTESIAN_POINT('Ctrl Pts',(-40.4639642811328,214.995967593475,29.3991082141453));
#2507=CARTESIAN_POINT('Ctrl Pts',(-45.1203255816707,214.495967593475,22.990245878166));
#2508=CARTESIAN_POINT('Ctrl Pts',(-47.5683409623447,213.995967593475,15.4561608176784));
#2509=CARTESIAN_POINT('Ctrl Pts',(-50.0163563430187,213.495967593475,7.9220757571907));
#2510=CARTESIAN_POINT('Ctrl Pts',(-50.0163970020424,212.995967593475,0.000256710972403907));
#2511=CARTESIAN_POINT('Ctrl Pts',(-50.0164376610661,212.495967593475,-7.92156233524589));
#2512=CARTESIAN_POINT('Ctrl Pts',(-47.5684996184509,211.995967593475,-15.4556725243922));
#2513=CARTESIAN_POINT('Ctrl Pts',(-45.1205615758357,211.495967593475,-22.9897827135384));
#2514=CARTESIAN_POINT('Ctrl Pts',(-40.4642660629801,210.995967593475,-29.3986928470667));
#2515=CARTESIAN_POINT('Ctrl Pts',(-35.8079705501245,210.495967593475,-35.8076029805949));
#2516=CARTESIAN_POINT('Ctrl Pts',(-29.3991082141453,209.995967593475,-40.4639642811328));
#2517=CARTESIAN_POINT('Ctrl Pts',(-22.9902458781661,209.495967593475,-45.1203255816707));
#2518=CARTESIAN_POINT('Ctrl Pts',(-15.4561608176784,208.995967593475,-47.5683409623447));
#2519=CARTESIAN_POINT('Ctrl Pts',(-7.92207575719071,208.495967593475,-50.0163563430187));
#2520=CARTESIAN_POINT('Ctrl Pts',(-0.00025671097240697,207.995967593475,
-50.0163970020424));
#2521=CARTESIAN_POINT('Ctrl Pts',(7.92156233524589,207.495967593475,-50.0164376610661));
#2522=CARTESIAN_POINT('Ctrl Pts',(15.4556725243922,206.995967593475,-47.5684996184509));
#2523=CARTESIAN_POINT('Ctrl Pts',(22.9897827135384,206.495967593475,-45.1205615758357));
#2524=CARTESIAN_POINT('Ctrl Pts',(29.3986928470667,205.995967593475,-40.4642660629801));
#2525=CARTESIAN_POINT('Ctrl Pts',(35.8076029805949,205.495967593475,-35.8079705501245));
#2526=CARTESIAN_POINT('Ctrl Pts',(40.4639642811328,204.995967593475,-29.3991082141453));
#2527=CARTESIAN_POINT('Ctrl Pts',(45.1203255816707,204.495967593475,-22.9902458781661));
#2528=CARTESIAN_POINT('Ctrl Pts',(47.5683409623447,203.995967593475,-15.4561608176784));
#2529=CARTESIAN_POINT('Ctrl Pts',(50.0163563430187,203.495967593475,-7.92207575719071));
#2530=CARTESIAN_POINT('Ctrl Pts',(50.0163970020424,202.995967593475,-0.000256710972410033));
#2531=CARTESIAN_POINT('Ctrl Pts',(50.0164376610661,202.495967593475,7.92156233524589));
#2532=CARTESIAN_POINT('Ctrl Pts',(47.5684996184509,201.995967593475,15.4556725243922));
#2533=CARTESIAN_POINT('Ctrl Pts',(45.1205615758358,201.495967593475,22.9897827135384));
#2534=CARTESIAN_POINT('Ctrl Pts',(40.4642660629801,200.995967593475,29.3986928470667));
#2535=CARTESIAN_POINT('Ctrl Pts',(35.8079705501245,200.495967593475,35.8076029805949));
#2536=CARTESIAN_POINT('Ctrl Pts',(29.3991082141453,199.995967593475,40.4639642811328));
#2537=CARTESIAN_POINT('Ctrl Pts',(22.9902458781661,199.495967593475,45.1203255816707));
#2538=CARTESIAN_POINT('Ctrl Pts',(15.4561608176784,198.995967593475,47.5683409623447));
#2539=CARTESIAN_POINT('Ctrl Pts',(7.92207575719071,198.495967593475,50.0163563430187));
#2540=CARTESIAN_POINT('Ctrl Pts',(0.000256710972400845,197.995967593475,
50.0163970020424));
#2541=CARTESIAN_POINT('Ctrl Pts',(-7.92156233524589,197.495967593475,50.0164376610661));
#2542=CARTESIAN_POINT('Ctrl Pts',(-15.4556725243922,196.995967593475,47.5684996184509));
#2543=CARTESIAN_POINT('Ctrl Pts',(-22.9897827135384,196.495967593475,45.1205615758357));
#2544=CARTESIAN_POINT('Ctrl Pts',(-29.3986928470667,195.995967593475,40.4642660629801));
#2545=CARTESIAN_POINT('Ctrl Pts',(-35.8076029805949,195.495967593475,35.8079705501245));
#2546=CARTESIAN_POINT('Ctrl Pts',(-40.4639642811328,194.995967593475,29.3991082141453));
#2547=CARTESIAN_POINT('Ctrl Pts',(-45.1203255816707,194.495967593475,22.990245878166));
#2548=CARTESIAN_POINT('Ctrl Pts',(-47.5683409623447,193.995967593475,15.4561608176784));
#2549=CARTESIAN_POINT('Ctrl Pts',(-50.0163563430187,193.495967593475,7.9220757571907));
#2550=CARTESIAN_POINT('Ctrl Pts',(-50.0163970020424,192.995967593475,0.000256710972403907));
#2551=CARTESIAN_POINT('Ctrl Pts',(-50.0164376610661,192.495967593475,-7.92156233524589));
#2552=CARTESIAN_POINT('Ctrl Pts',(-47.5684996184509,191.995967593475,-15.4556725243922));
#2553=CARTESIAN_POINT('Ctrl Pts',(-45.1205615758357,191.495967593475,-22.9897827135384));
#2554=CARTESIAN_POINT('Ctrl Pts',(-40.4642660629801,190.995967593475,-29.3986928470667));
#2555=CARTESIAN_POINT('Ctrl Pts',(-35.8079705501245,190.495967593475,-35.8076029805949));
#2556=CARTESIAN_POINT('Ctrl Pts',(-29.3991082141453,189.995967593475,-40.4639642811328));
#2557=CARTESIAN_POINT('Ctrl Pts',(-22.9902458781661,189.495967593475,-45.1203255816707));
#2558=CARTESIAN_POINT('Ctrl Pts',(-15.4561608176784,188.995967593475,-47.5683409623447));
#2559=CARTESIAN_POINT('Ctrl Pts',(-7.92207575719071,188.495967593475,-50.0163563430187));
#2560=CARTESIAN_POINT('Ctrl Pts',(-0.00025671097240697,187.995967593475,
-50.0163970020424));
#2561=CARTESIAN_POINT('Ctrl Pts',(7.92156233524589,187.495967593475,-50.0164376610661));
#2562=CARTESIAN_POINT('Ctrl Pts',(15.4556725243922,186.995967593475,-47.5684996184509));
#2563=CARTESIAN_POINT('Ctrl Pts',(22.9897827135384,186.495967593475,-45.1205615758357));
#2564=CARTESIAN_POINT('Ctrl Pts',(29.3986928470667,185.995967593475,-40.4642660629801));
#2565=CARTESIAN_POINT('Ctrl Pts',(35.8076029805949,185.495967593475,-35.8079705501245));
#2566=CARTESIAN_POINT('Ctrl Pts',(40.4639642811328,184.995967593475,-29.3991082141453));
#2567=CARTESIAN_POINT('Ctrl Pts',(45.1203255816707,184.495967593475,-22.9902458781661));
#2568=CARTESIAN_POINT('Ctrl Pts',(47.5683409623447,183.995967593475,-15.4561608176784));
#2569=CARTESIAN_POINT('Ctrl Pts',(50.0163563430187,183.495967593475,-7.92207575719071));
#2570=CARTESIAN_POINT('Ctrl Pts',(50.0163970020424,182.995967593475,-0.000256710972410033));
#2571=CARTESIAN_POINT('Ctrl Pts',(50.0164376610661,182.495967593475,7.92156233524589));
#2572=CARTESIAN_POINT('Ctrl Pts',(47.5684996184509,181.995967593475,15.4556725243922));
#2573=CARTESIAN_POINT('Ctrl Pts',(45.1205615758358,181.495967593475,22.9897827135384));
#2574=CARTESIAN_POINT('Ctrl Pts',(40.4642660629801,180.995967593475,29.3986928470667));
#2575=CARTESIAN_POINT('Ctrl Pts',(35.8079705501245,180.495967593475,35.8076029805949));
#2576=CARTESIAN_POINT('Ctrl Pts',(29.3991082141453,179.995967593475,40.4639642811328));
#2577=CARTESIAN_POINT('Ctrl Pts',(22.9902458781661,179.495967593475,45.1203255816707));
#2578=CARTESIAN_POINT('Ctrl Pts',(15.4561608176784,178.995967593475,47.5683409623447));
#2579=CARTESIAN_POINT('Ctrl Pts',(7.92207575719071,178.495967593475,50.0163563430187));
#2580=CARTESIAN_POINT('Ctrl Pts',(0.000256710972400845,177.995967593475,
50.0163970020424));
#2581=CARTESIAN_POINT('Ctrl Pts',(0.190856796705285,235.002028447915,50.0163970020424));
#2582=CARTESIAN_POINT('Ctrl Pts',(-7.73096224951301,234.502028447915,50.0466257489707));
#2583=CARTESIAN_POINT('Ctrl Pts',(-15.2744010708495,234.002028447915,47.6273982840717));
#2584=CARTESIAN_POINT('Ctrl Pts',(-22.817839892186,233.502028447915,45.2081708191727));
#2585=CARTESIAN_POINT('Ctrl Pts',(-29.2444941385794,233.002028447915,40.5762979824596));
#2586=CARTESIAN_POINT('Ctrl Pts',(-35.6711483849729,232.502028447915,35.9444251457465));
#2587=CARTESIAN_POINT('Ctrl Pts',(-40.3519323616533,232.002028447915,29.5533069226325));
#2588=CARTESIAN_POINT('Ctrl Pts',(-45.0327163383337,231.502028447915,23.1621886995185));
#2589=CARTESIAN_POINT('Ctrl Pts',(-47.5094422967239,231.002028447915,15.6374322712211));
#2590=CARTESIAN_POINT('Ctrl Pts',(-49.9861682551141,230.502028447915,8.11267584292358));
#2591=CARTESIAN_POINT('Ctrl Pts',(-50.0163970020424,230.002028447915,0.190856796705288));
#2592=CARTESIAN_POINT('Ctrl Pts',(-50.0466257489707,229.502028447915,-7.73096224951301));
#2593=CARTESIAN_POINT('Ctrl Pts',(-47.6273982840717,229.002028447915,-15.2744010708495));
#2594=CARTESIAN_POINT('Ctrl Pts',(-45.2081708191727,228.502028447915,-22.817839892186));
#2595=CARTESIAN_POINT('Ctrl Pts',(-40.5762979824596,228.002028447915,-29.2444941385794));
#2596=CARTESIAN_POINT('Ctrl Pts',(-35.9444251457465,227.502028447915,-35.6711483849729));
#2597=CARTESIAN_POINT('Ctrl Pts',(-29.5533069226325,227.002028447915,-40.3519323616533));
#2598=CARTESIAN_POINT('Ctrl Pts',(-23.1621886995185,226.502028447915,-45.0327163383337));
#2599=CARTESIAN_POINT('Ctrl Pts',(-15.6374322712211,226.002028447915,-47.5094422967239));
#2600=CARTESIAN_POINT('Ctrl Pts',(-8.11267584292359,225.502028447915,-49.9861682551141));
#2601=CARTESIAN_POINT('Ctrl Pts',(-0.190856796705292,225.002028447915,-50.0163970020424));
#2602=CARTESIAN_POINT('Ctrl Pts',(7.730962249513,224.502028447915,-50.0466257489707));
#2603=CARTESIAN_POINT('Ctrl Pts',(15.2744010708495,224.002028447915,-47.6273982840717));
#2604=CARTESIAN_POINT('Ctrl Pts',(22.817839892186,223.502028447915,-45.2081708191727));
#2605=CARTESIAN_POINT('Ctrl Pts',(29.2444941385794,223.002028447915,-40.5762979824596));
#2606=CARTESIAN_POINT('Ctrl Pts',(35.6711483849729,222.502028447915,-35.9444251457465));
#2607=CARTESIAN_POINT('Ctrl Pts',(40.3519323616533,222.002028447915,-29.5533069226325));
#2608=CARTESIAN_POINT('Ctrl Pts',(45.0327163383337,221.502028447915,-23.1621886995185));
#2609=CARTESIAN_POINT('Ctrl Pts',(47.5094422967239,221.002028447915,-15.6374322712211));
#2610=CARTESIAN_POINT('Ctrl Pts',(49.9861682551141,220.502028447915,-8.11267584292359));
#2611=CARTESIAN_POINT('Ctrl Pts',(50.0163970020424,220.002028447915,-0.190856796705295));
#2612=CARTESIAN_POINT('Ctrl Pts',(50.0466257489707,219.502028447915,7.730962249513));
#2613=CARTESIAN_POINT('Ctrl Pts',(47.6273982840717,219.002028447915,15.2744010708495));
#2614=CARTESIAN_POINT('Ctrl Pts',(45.2081708191727,218.502028447915,22.817839892186));
#2615=CARTESIAN_POINT('Ctrl Pts',(40.5762979824596,218.002028447915,29.2444941385794));
#2616=CARTESIAN_POINT('Ctrl Pts',(35.9444251457465,217.502028447915,35.6711483849729));
#2617=CARTESIAN_POINT('Ctrl Pts',(29.5533069226325,217.002028447915,40.3519323616533));
#2618=CARTESIAN_POINT('Ctrl Pts',(23.1621886995185,216.502028447915,45.0327163383337));
#2619=CARTESIAN_POINT('Ctrl Pts',(15.6374322712211,216.002028447915,47.5094422967239));
#2620=CARTESIAN_POINT('Ctrl Pts',(8.11267584292359,215.502028447915,49.9861682551141));
#2621=CARTESIAN_POINT('Ctrl Pts',(0.190856796705285,215.002028447915,50.0163970020424));
#2622=CARTESIAN_POINT('Ctrl Pts',(-7.73096224951301,214.502028447915,50.0466257489707));
#2623=CARTESIAN_POINT('Ctrl Pts',(-15.2744010708495,214.002028447915,47.6273982840717));
#2624=CARTESIAN_POINT('Ctrl Pts',(-22.817839892186,213.502028447915,45.2081708191727));
#2625=CARTESIAN_POINT('Ctrl Pts',(-29.2444941385794,213.002028447915,40.5762979824596));
#2626=CARTESIAN_POINT('Ctrl Pts',(-35.6711483849729,212.502028447915,35.9444251457465));
#2627=CARTESIAN_POINT('Ctrl Pts',(-40.3519323616533,212.002028447915,29.5533069226325));
#2628=CARTESIAN_POINT('Ctrl Pts',(-45.0327163383337,211.502028447915,23.1621886995185));
#2629=CARTESIAN_POINT('Ctrl Pts',(-47.5094422967239,211.002028447915,15.6374322712211));
#2630=CARTESIAN_POINT('Ctrl Pts',(-49.9861682551141,210.502028447915,8.11267584292358));
#2631=CARTESIAN_POINT('Ctrl Pts',(-50.0163970020424,210.002028447915,0.190856796705288));
#2632=CARTESIAN_POINT('Ctrl Pts',(-50.0466257489707,209.502028447915,-7.73096224951301));
#2633=CARTESIAN_POINT('Ctrl Pts',(-47.6273982840717,209.002028447915,-15.2744010708495));
#2634=CARTESIAN_POINT('Ctrl Pts',(-45.2081708191727,208.502028447915,-22.817839892186));
#2635=CARTESIAN_POINT('Ctrl Pts',(-40.5762979824596,208.002028447915,-29.2444941385794));
#2636=CARTESIAN_POINT('Ctrl Pts',(-35.9444251457465,207.502028447915,-35.6711483849729));
#2637=CARTESIAN_POINT('Ctrl Pts',(-29.5533069226325,207.002028447915,-40.3519323616533));
#2638=CARTESIAN_POINT('Ctrl Pts',(-23.1621886995185,206.502028447915,-45.0327163383337));
#2639=CARTESIAN_POINT('Ctrl Pts',(-15.6374322712211,206.002028447915,-47.5094422967239));
#2640=CARTESIAN_POINT('Ctrl Pts',(-8.11267584292359,205.502028447915,-49.9861682551141));
#2641=CARTESIAN_POINT('Ctrl Pts',(-0.190856796705292,205.002028447915,-50.0163970020424));
#2642=CARTESIAN_POINT('Ctrl Pts',(7.730962249513,204.502028447915,-50.0466257489707));
#2643=CARTESIAN_POINT('Ctrl Pts',(15.2744010708495,204.002028447915,-47.6273982840717));
#2644=CARTESIAN_POINT('Ctrl Pts',(22.817839892186,203.502028447915,-45.2081708191727));
#2645=CARTESIAN_POINT('Ctrl Pts',(29.2444941385794,203.002028447915,-40.5762979824596));
#2646=CARTESIAN_POINT('Ctrl Pts',(35.6711483849729,202.502028447915,-35.9444251457465));
#2647=CARTESIAN_POINT('Ctrl Pts',(40.3519323616533,202.002028447915,-29.5533069226325));
#2648=CARTESIAN_POINT('Ctrl Pts',(45.0327163383337,201.502028447915,-23.1621886995185));
#2649=CARTESIAN_POINT('Ctrl Pts',(47.5094422967239,201.002028447915,-15.6374322712211));
#2650=CARTESIAN_POINT('Ctrl Pts',(49.9861682551141,200.502028447915,-8.11267584292359));
#2651=CARTESIAN_POINT('Ctrl Pts',(50.0163970020424,200.002028447915,-0.190856796705295));
#2652=CARTESIAN_POINT('Ctrl Pts',(50.0466257489707,199.502028447915,7.730962249513));
#2653=CARTESIAN_POINT('Ctrl Pts',(47.6273982840717,199.002028447915,15.2744010708495));
#2654=CARTESIAN_POINT('Ctrl Pts',(45.2081708191727,198.502028447915,22.817839892186));
#2655=CARTESIAN_POINT('Ctrl Pts',(40.5762979824596,198.002028447915,29.2444941385794));
#2656=CARTESIAN_POINT('Ctrl Pts',(35.9444251457465,197.502028447915,35.6711483849729));
#2657=CARTESIAN_POINT('Ctrl Pts',(29.5533069226325,197.002028447915,40.3519323616533));
#2658=CARTESIAN_POINT('Ctrl Pts',(23.1621886995185,196.502028447915,45.0327163383337));
#2659=CARTESIAN_POINT('Ctrl Pts',(15.6374322712211,196.002028447915,47.5094422967239));
#2660=CARTESIAN_POINT('Ctrl Pts',(8.11267584292359,195.502028447915,49.9861682551141));
#2661=CARTESIAN_POINT('Ctrl Pts',(0.190856796705285,195.002028447915,50.0163970020424));
#2662=CARTESIAN_POINT('Ctrl Pts',(-7.73096224951301,194.502028447915,50.0466257489707));
#2663=CARTESIAN_POINT('Ctrl Pts',(-15.2744010708495,194.002028447915,47.6273982840717));
#2664=CARTESIAN_POINT('Ctrl Pts',(-22.817839892186,193.502028447915,45.2081708191727));
#2665=CARTESIAN_POINT('Ctrl Pts',(-29.2444941385794,193.002028447915,40.5762979824596));
#2666=CARTESIAN_POINT('Ctrl Pts',(-35.6711483849729,192.502028447915,35.9444251457465));
#2667=CARTESIAN_POINT('Ctrl Pts',(-40.3519323616533,192.002028447915,29.5533069226325));
#2668=CARTESIAN_POINT('Ctrl Pts',(-45.0327163383337,191.502028447915,23.1621886995185));
#2669=CARTESIAN_POINT('Ctrl Pts',(-47.5094422967239,191.002028447915,15.6374322712211));
#2670=CARTESIAN_POINT('Ctrl Pts',(-49.9861682551141,190.502028447915,8.11267584292358));
#2671=CARTESIAN_POINT('Ctrl Pts',(-50.0163970020424,190.002028447915,0.190856796705288));
#2672=CARTESIAN_POINT('Ctrl Pts',(-50.0466257489707,189.502028447915,-7.73096224951301));
#2673=CARTESIAN_POINT('Ctrl Pts',(-47.6273982840717,189.002028447915,-15.2744010708495));
#2674=CARTESIAN_POINT('Ctrl Pts',(-45.2081708191727,188.502028447915,-22.817839892186));
#2675=CARTESIAN_POINT('Ctrl Pts',(-40.5762979824596,188.002028447915,-29.2444941385794));
#2676=CARTESIAN_POINT('Ctrl Pts',(-35.9444251457465,187.502028447915,-35.6711483849729));
#2677=CARTESIAN_POINT('Ctrl Pts',(-29.5533069226325,187.002028447915,-40.3519323616533));
#2678=CARTESIAN_POINT('Ctrl Pts',(-23.1621886995185,186.502028447915,-45.0327163383337));
#2679=CARTESIAN_POINT('Ctrl Pts',(-15.6374322712211,186.002028447915,-47.5094422967239));
#2680=CARTESIAN_POINT('Ctrl Pts',(-8.11267584292359,185.502028447915,-49.9861682551141));
#2681=CARTESIAN_POINT('Ctrl Pts',(-0.190856796705292,185.002028447915,-50.0163970020424));
#2682=CARTESIAN_POINT('Ctrl Pts',(7.730962249513,184.502028447915,-50.0466257489707));
#2683=CARTESIAN_POINT('Ctrl Pts',(15.2744010708495,184.002028447915,-47.6273982840717));
#2684=CARTESIAN_POINT('Ctrl Pts',(22.817839892186,183.502028447915,-45.2081708191727));
#2685=CARTESIAN_POINT('Ctrl Pts',(29.2444941385794,183.002028447915,-40.5762979824596));
#2686=CARTESIAN_POINT('Ctrl Pts',(35.6711483849729,182.502028447915,-35.9444251457465));
#2687=CARTESIAN_POINT('Ctrl Pts',(40.3519323616533,182.002028447915,-29.5533069226325));
#2688=CARTESIAN_POINT('Ctrl Pts',(45.0327163383337,181.502028447915,-23.1621886995185));
#2689=CARTESIAN_POINT('Ctrl Pts',(47.5094422967239,181.002028447915,-15.6374322712211));
#2690=CARTESIAN_POINT('Ctrl Pts',(49.9861682551141,180.502028447915,-8.11267584292359));
#2691=CARTESIAN_POINT('Ctrl Pts',(50.0163970020424,180.002028447915,-0.190856796705295));
#2692=CARTESIAN_POINT('Ctrl Pts',(50.0466257489707,179.502028447915,7.730962249513));
#2693=CARTESIAN_POINT('Ctrl Pts',(47.6273982840717,179.002028447915,15.2744010708495));
#2694=CARTESIAN_POINT('Ctrl Pts',(45.2081708191727,178.502028447915,22.817839892186));
#2695=CARTESIAN_POINT('Ctrl Pts',(40.5762979824596,178.002028447915,29.2444941385794));
#2696=CARTESIAN_POINT('Ctrl Pts',(35.9444251457465,177.502028447915,35.6711483849729));
#2697=CARTESIAN_POINT('Ctrl Pts',(29.5533069226325,177.002028447915,40.3519323616533));
#2698=CARTESIAN_POINT('Ctrl Pts',(23.1621886995185,176.502028447915,45.0327163383337));
#2699=CARTESIAN_POINT('Ctrl Pts',(15.6374322712211,176.002028447915,47.5094422967239));
#2700=CARTESIAN_POINT('Ctrl Pts',(8.11267584292359,175.502028447915,49.9861682551141));
#2701=CARTESIAN_POINT('Ctrl Pts',(0.190856796705285,175.002028447915,50.0163970020424));
#2702=CARTESIAN_POINT('Ctrl Pts',(0.000256710972400845,237.995967593475,
50.0163970020424));
#2703=CARTESIAN_POINT('Ctrl Pts',(-7.92156233524589,237.495967593475,50.0164376610661));
#2704=CARTESIAN_POINT('Ctrl Pts',(-15.4556725243922,236.995967593475,47.5684996184509));
#2705=CARTESIAN_POINT('Ctrl Pts',(-22.9897827135384,236.495967593475,45.1205615758357));
#2706=CARTESIAN_POINT('Ctrl Pts',(-29.3986928470667,235.995967593475,40.4642660629801));
#2707=CARTESIAN_POINT('Ctrl Pts',(-35.8076029805949,235.495967593475,35.8079705501245));
#2708=CARTESIAN_POINT('Ctrl Pts',(-40.4639642811328,234.995967593475,29.3991082141453));
#2709=CARTESIAN_POINT('Ctrl Pts',(-45.1203255816707,234.495967593475,22.990245878166));
#2710=CARTESIAN_POINT('Ctrl Pts',(-47.5683409623447,233.995967593475,15.4561608176784));
#2711=CARTESIAN_POINT('Ctrl Pts',(-50.0163563430187,233.495967593475,7.9220757571907));
#2712=CARTESIAN_POINT('Ctrl Pts',(-50.0163970020424,232.995967593475,0.000256710972403907));
#2713=CARTESIAN_POINT('Ctrl Pts',(-50.0164376610661,232.495967593475,-7.92156233524589));
#2714=CARTESIAN_POINT('Ctrl Pts',(-47.5684996184509,231.995967593475,-15.4556725243922));
#2715=CARTESIAN_POINT('Ctrl Pts',(-45.1205615758357,231.495967593475,-22.9897827135384));
#2716=CARTESIAN_POINT('Ctrl Pts',(-40.4642660629801,230.995967593475,-29.3986928470667));
#2717=CARTESIAN_POINT('Ctrl Pts',(-35.8079705501245,230.495967593475,-35.8076029805949));
#2718=CARTESIAN_POINT('Ctrl Pts',(-29.3991082141453,229.995967593475,-40.4639642811328));
#2719=CARTESIAN_POINT('Ctrl Pts',(-22.9902458781661,229.495967593475,-45.1203255816707));
#2720=CARTESIAN_POINT('Ctrl Pts',(-15.4561608176784,228.995967593475,-47.5683409623447));
#2721=CARTESIAN_POINT('Ctrl Pts',(-7.92207575719071,228.495967593475,-50.0163563430187));
#2722=CARTESIAN_POINT('Ctrl Pts',(-0.00025671097240697,227.995967593475,
-50.0163970020424));
#2723=CARTESIAN_POINT('Ctrl Pts',(7.92156233524589,227.495967593475,-50.0164376610661));
#2724=CARTESIAN_POINT('Ctrl Pts',(15.4556725243922,226.995967593475,-47.5684996184509));
#2725=CARTESIAN_POINT('Ctrl Pts',(22.9897827135384,226.495967593475,-45.1205615758357));
#2726=CARTESIAN_POINT('Ctrl Pts',(29.3986928470667,225.995967593475,-40.4642660629801));
#2727=CARTESIAN_POINT('Ctrl Pts',(35.8076029805949,225.495967593475,-35.8079705501245));
#2728=CARTESIAN_POINT('Ctrl Pts',(40.4639642811328,224.995967593475,-29.3991082141453));
#2729=CARTESIAN_POINT('Ctrl Pts',(45.1203255816707,224.495967593475,-22.9902458781661));
#2730=CARTESIAN_POINT('Ctrl Pts',(47.5683409623447,223.995967593475,-15.4561608176784));
#2731=CARTESIAN_POINT('Ctrl Pts',(50.0163563430187,223.495967593475,-7.92207575719071));
#2732=CARTESIAN_POINT('Ctrl Pts',(50.0163970020424,222.995967593475,-0.000256710972410033));
#2733=CARTESIAN_POINT('Ctrl Pts',(50.0164376610661,222.495967593475,7.92156233524589));
#2734=CARTESIAN_POINT('Ctrl Pts',(47.5684996184509,221.995967593475,15.4556725243922));
#2735=CARTESIAN_POINT('Ctrl Pts',(45.1205615758358,221.495967593475,22.9897827135384));
#2736=CARTESIAN_POINT('Ctrl Pts',(40.4642660629801,220.995967593475,29.3986928470667));
#2737=CARTESIAN_POINT('Ctrl Pts',(35.8079705501245,220.495967593475,35.8076029805949));
#2738=CARTESIAN_POINT('Ctrl Pts',(29.3991082141453,219.995967593475,40.4639642811328));
#2739=CARTESIAN_POINT('Ctrl Pts',(22.9902458781661,219.495967593475,45.1203255816707));
#2740=CARTESIAN_POINT('Ctrl Pts',(15.4561608176784,218.995967593475,47.5683409623447));
#2741=CARTESIAN_POINT('Ctrl Pts',(7.92207575719071,218.495967593475,50.0163563430187));
#2742=CARTESIAN_POINT('Ctrl Pts',(0.000256710972400845,217.995967593475,
50.0163970020424));
#2743=CARTESIAN_POINT('Ctrl Pts',(-7.92156233524589,217.495967593475,50.0164376610661));
#2744=CARTESIAN_POINT('Ctrl Pts',(-15.4556725243922,216.995967593475,47.5684996184509));
#2745=CARTESIAN_POINT('Ctrl Pts',(-22.9897827135384,216.495967593475,45.1205615758357));
#2746=CARTESIAN_POINT('Ctrl Pts',(-29.3986928470667,215.995967593475,40.4642660629801));
#2747=CARTESIAN_POINT('Ctrl Pts',(-35.8076029805949,215.495967593475,35.8079705501245));
#2748=CARTESIAN_POINT('Ctrl Pts',(-40.4639642811328,214.995967593475,29.3991082141453));
#2749=CARTESIAN_POINT('Ctrl Pts',(-45.1203255816707,214.495967593475,22.990245878166));
#2750=CARTESIAN_POINT('Ctrl Pts',(-47.5683409623447,213.995967593475,15.4561608176784));
#2751=CARTESIAN_POINT('Ctrl Pts',(-50.0163563430187,213.495967593475,7.9220757571907));
#2752=CARTESIAN_POINT('Ctrl Pts',(-50.0163970020424,212.995967593475,0.000256710972403907));
#2753=CARTESIAN_POINT('Ctrl Pts',(-50.0164376610661,212.495967593475,-7.92156233524589));
#2754=CARTESIAN_POINT('Ctrl Pts',(-47.5684996184509,211.995967593475,-15.4556725243922));
#2755=CARTESIAN_POINT('Ctrl Pts',(-45.1205615758357,211.495967593475,-22.9897827135384));
#2756=CARTESIAN_POINT('Ctrl Pts',(-40.4642660629801,210.995967593475,-29.3986928470667));
#2757=CARTESIAN_POINT('Ctrl Pts',(-35.8079705501245,210.495967593475,-35.8076029805949));
#2758=CARTESIAN_POINT('Ctrl Pts',(-29.3991082141453,209.995967593475,-40.4639642811328));
#2759=CARTESIAN_POINT('Ctrl Pts',(-22.9902458781661,209.495967593475,-45.1203255816707));
#2760=CARTESIAN_POINT('Ctrl Pts',(-15.4561608176784,208.995967593475,-47.5683409623447));
#2761=CARTESIAN_POINT('Ctrl Pts',(-7.92207575719071,208.495967593475,-50.0163563430187));
#2762=CARTESIAN_POINT('Ctrl Pts',(-0.00025671097240697,207.995967593475,
-50.0163970020424));
#2763=CARTESIAN_POINT('Ctrl Pts',(7.92156233524589,207.495967593475,-50.0164376610661));
#2764=CARTESIAN_POINT('Ctrl Pts',(15.4556725243922,206.995967593475,-47.5684996184509));
#2765=CARTESIAN_POINT('Ctrl Pts',(22.9897827135384,206.495967593475,-45.1205615758357));
#2766=CARTESIAN_POINT('Ctrl Pts',(29.3986928470667,205.995967593475,-40.4642660629801));
#2767=CARTESIAN_POINT('Ctrl Pts',(35.8076029805949,205.495967593475,-35.8079705501245));
#2768=CARTESIAN_POINT('Ctrl Pts',(40.4639642811328,204.995967593475,-29.3991082141453));
#2769=CARTESIAN_POINT('Ctrl Pts',(45.1203255816707,204.495967593475,-22.9902458781661));
#2770=CARTESIAN_POINT('Ctrl Pts',(47.5683409623447,203.995967593475,-15.4561608176784));
#2771=CARTESIAN_POINT('Ctrl Pts',(50.0163563430187,203.495967593475,-7.92207575719071));
#2772=CARTESIAN_POINT('Ctrl Pts',(50.0163970020424,202.995967593475,-0.000256710972410033));
#2773=CARTESIAN_POINT('Ctrl Pts',(50.0164376610661,202.495967593475,7.92156233524589));
#2774=CARTESIAN_POINT('Ctrl Pts',(47.5684996184509,201.995967593475,15.4556725243922));
#2775=CARTESIAN_POINT('Ctrl Pts',(45.1205615758358,201.495967593475,22.9897827135384));
#2776=CARTESIAN_POINT('Ctrl Pts',(40.4642660629801,200.995967593475,29.3986928470667));
#2777=CARTESIAN_POINT('Ctrl Pts',(35.8079705501245,200.495967593475,35.8076029805949));
#2778=CARTESIAN_POINT('Ctrl Pts',(29.3991082141453,199.995967593475,40.4639642811328));
#2779=CARTESIAN_POINT('Ctrl Pts',(22.9902458781661,199.495967593475,45.1203255816707));
#2780=CARTESIAN_POINT('Ctrl Pts',(15.4561608176784,198.995967593475,47.5683409623447));
#2781=CARTESIAN_POINT('Ctrl Pts',(7.92207575719071,198.495967593475,50.0163563430187));
#2782=CARTESIAN_POINT('Ctrl Pts',(0.000256710972400845,197.995967593475,
50.0163970020424));
#2783=CARTESIAN_POINT('Ctrl Pts',(-7.92156233524589,197.495967593475,50.0164376610661));
#2784=CARTESIAN_POINT('Ctrl Pts',(-15.4556725243922,196.995967593475,47.5684996184509));
#2785=CARTESIAN_POINT('Ctrl Pts',(-22.9897827135384,196.495967593475,45.1205615758357));
#2786=CARTESIAN_POINT('Ctrl Pts',(-29.3986928470667,195.995967593475,40.4642660629801));
#2787=CARTESIAN_POINT('Ctrl Pts',(-35.8076029805949,195.495967593475,35.8079705501245));
#2788=CARTESIAN_POINT('Ctrl Pts',(-40.4639642811328,194.995967593475,29.3991082141453));
#2789=CARTESIAN_POINT('Ctrl Pts',(-45.1203255816707,194.495967593475,22.990245878166));
#2790=CARTESIAN_POINT('Ctrl Pts',(-47.5683409623447,193.995967593475,15.4561608176784));
#2791=CARTESIAN_POINT('Ctrl Pts',(-50.0163563430187,193.495967593475,7.9220757571907));
#2792=CARTESIAN_POINT('Ctrl Pts',(-50.0163970020424,192.995967593475,0.000256710972403907));
#2793=CARTESIAN_POINT('Ctrl Pts',(-50.0164376610661,192.495967593475,-7.92156233524589));
#2794=CARTESIAN_POINT('Ctrl Pts',(-47.5684996184509,191.995967593475,-15.4556725243922));
#2795=CARTESIAN_POINT('Ctrl Pts',(-45.1205615758357,191.495967593475,-22.9897827135384));
#2796=CARTESIAN_POINT('Ctrl Pts',(-40.4642660629801,190.995967593475,-29.3986928470667));
#2797=CARTESIAN_POINT('Ctrl Pts',(-35.8079705501245,190.495967593475,-35.8076029805949));
#2798=CARTESIAN_POINT('Ctrl Pts',(-29.3991082141453,189.995967593475,-40.4639642811328));
#2799=CARTESIAN_POINT('Ctrl Pts',(-22.9902458781661,189.495967593475,-45.1203255816707));
#2800=CARTESIAN_POINT('Ctrl Pts',(-15.4561608176784,188.995967593475,-47.5683409623447));
#2801=CARTESIAN_POINT('Ctrl Pts',(-7.92207575719071,188.495967593475,-50.0163563430187));
#2802=CARTESIAN_POINT('Ctrl Pts',(-0.00025671097240697,187.995967593475,
-50.0163970020424));
#2803=CARTESIAN_POINT('Ctrl Pts',(7.92156233524589,187.495967593475,-50.0164376610661));
#2804=CARTESIAN_POINT('Ctrl Pts',(15.4556725243922,186.995967593475,-47.5684996184509));
#2805=CARTESIAN_POINT('Ctrl Pts',(22.9897827135384,186.495967593475,-45.1205615758357));
#2806=CARTESIAN_POINT('Ctrl Pts',(29.3986928470667,185.995967593475,-40.4642660629801));
#2807=CARTESIAN_POINT('Ctrl Pts',(35.8076029805949,185.495967593475,-35.8079705501245));
#2808=CARTESIAN_POINT('Ctrl Pts',(40.4639642811328,184.995967593475,-29.3991082141453));
#2809=CARTESIAN_POINT('Ctrl Pts',(45.1203255816707,184.495967593475,-22.9902458781661));
#2810=CARTESIAN_POINT('Ctrl Pts',(47.5683409623447,183.995967593475,-15.4561608176784));
#2811=CARTESIAN_POINT('Ctrl Pts',(50.0163563430187,183.495967593475,-7.92207575719071));
#2812=CARTESIAN_POINT('Ctrl Pts',(50.0163970020424,182.995967593475,-0.000256710972410033));
#2813=CARTESIAN_POINT('Ctrl Pts',(50.0164376610661,182.495967593475,7.92156233524589));
#2814=CARTESIAN_POINT('Ctrl Pts',(47.5684996184509,181.995967593475,15.4556725243922));
#2815=CARTESIAN_POINT('Ctrl Pts',(45.1205615758358,181.495967593475,22.9897827135384));
#2816=CARTESIAN_POINT('Ctrl Pts',(40.4642660629801,180.995967593475,29.3986928470667));
#2817=CARTESIAN_POINT('Ctrl Pts',(35.8079705501245,180.495967593475,35.8076029805949));
#2818=CARTESIAN_POINT('Ctrl Pts',(29.3991082141453,179.995967593475,40.4639642811328));
#2819=CARTESIAN_POINT('Ctrl Pts',(22.9902458781661,179.495967593475,45.1203255816707));
#2820=CARTESIAN_POINT('Ctrl Pts',(15.4561608176784,178.995967593475,47.5683409623447));
#2821=CARTESIAN_POINT('Ctrl Pts',(7.92207575719071,178.495967593475,50.0163563430187));
#2822=CARTESIAN_POINT('Ctrl Pts',(0.000256710972400845,177.995967593475,
50.0163970020424));
#2823=CARTESIAN_POINT('Origin',(0.,150.,0.));
#2824=CARTESIAN_POINT('',(-5.,100.,-24.4948974278318));
#2825=CARTESIAN_POINT('',(5.,100.,-24.4948974278318));
#2826=CARTESIAN_POINT('Origin',(0.,100.,0.));
#2827=CARTESIAN_POINT('',(5.,150.,-24.4948974278318));
#2828=CARTESIAN_POINT('',(5.,150.,-24.4948974278318));
#2829=CARTESIAN_POINT('',(-5.,150.,-24.4948974278318));
#2830=CARTESIAN_POINT('Origin',(0.,150.,0.));
#2831=CARTESIAN_POINT('',(-5.,150.,-24.4948974278318));
#2832=CARTESIAN_POINT('Origin',(5.,150.,-33.));
#2833=CARTESIAN_POINT('',(5.,100.,-33.));
#2834=CARTESIAN_POINT('',(5.,100.,-24.4948974278318));
#2835=CARTESIAN_POINT('',(5.,150.,-33.));
#2836=CARTESIAN_POINT('',(5.,150.,-33.));
#2837=CARTESIAN_POINT('',(5.,150.,-24.4948974278318));
#2838=CARTESIAN_POINT('Origin',(-5.,150.,-33.));
#2839=CARTESIAN_POINT('',(-5.,100.,-33.));
#2840=CARTESIAN_POINT('',(5.,100.,-33.));
#2841=CARTESIAN_POINT('',(-5.,150.,-33.));
#2842=CARTESIAN_POINT('',(-5.,150.,-33.));
#2843=CARTESIAN_POINT('',(5.,150.,-33.));
#2844=CARTESIAN_POINT('Origin',(-5.,150.,-33.));
#2845=CARTESIAN_POINT('',(-5.,100.,-33.));
#2846=CARTESIAN_POINT('',(-5.,150.,-33.));
#2847=CARTESIAN_POINT('Origin',(0.,150.,0.));
#2848=CARTESIAN_POINT('Origin',(0.,100.,0.));
#2849=CARTESIAN_POINT('',(275.,872.,6.11682576753421E-14));
#2850=CARTESIAN_POINT('',(275.,537.,-6.72205346941013E-15));
#2851=UNCERTAINTY_MEASURE_WITH_UNIT(LENGTH_MEASURE(0.01),#2859,
'DISTANCE_ACCURACY_VALUE',
'Maximum model space distance between geometric entities at asserted c
onnectivities');
#2852=UNCERTAINTY_MEASURE_WITH_UNIT(LENGTH_MEASURE(0.01),#2859,
'DISTANCE_ACCURACY_VALUE',
'Maximum model space distance between geometric entities at asserted c
onnectivities');
#2853=UNCERTAINTY_MEASURE_WITH_UNIT(LENGTH_MEASURE(0.01),#2859,
'DISTANCE_ACCURACY_VALUE',
'Maximum model space distance between geometric entities at asserted c
onnectivities');
#2854=UNCERTAINTY_MEASURE_WITH_UNIT(LENGTH_MEASURE(0.01),#2859,
'DISTANCE_ACCURACY_VALUE',
'Maximum model space distance between geometric entities at asserted c
onnectivities');
#2855=(
GEOMETRIC_REPRESENTATION_CONTEXT(3)
GLOBAL_UNCERTAINTY_ASSIGNED_CONTEXT((#2851))
GLOBAL_UNIT_ASSIGNED_CONTEXT((#2859,#2861,#2862))
REPRESENTATION_CONTEXT('','3D')
);
#2856=(
GEOMETRIC_REPRESENTATION_CONTEXT(3)
GLOBAL_UNCERTAINTY_ASSIGNED_CONTEXT((#2852))
GLOBAL_UNIT_ASSIGNED_CONTEXT((#2859,#2861,#2862))
REPRESENTATION_CONTEXT('','3D')
);
#2857=(
GEOMETRIC_REPRESENTATION_CONTEXT(3)
GLOBAL_UNCERTAINTY_ASSIGNED_CONTEXT((#2853))
GLOBAL_UNIT_ASSIGNED_CONTEXT((#2859,#2861,#2862))
REPRESENTATION_CONTEXT('','3D')
);
#2858=(
GEOMETRIC_REPRESENTATION_CONTEXT(3)
GLOBAL_UNCERTAINTY_ASSIGNED_CONTEXT((#2854))
GLOBAL_UNIT_ASSIGNED_CONTEXT((#2859,#2861,#2862))
REPRESENTATION_CONTEXT('','3D')
);
#2859=(
LENGTH_UNIT()
NAMED_UNIT(*)
SI_UNIT(.MILLI.,.METRE.)
);
#2860=(
LENGTH_UNIT()
NAMED_UNIT(*)
SI_UNIT($,.METRE.)
);
#2861=(
NAMED_UNIT(*)
PLANE_ANGLE_UNIT()
SI_UNIT($,.RADIAN.)
);
#2862=(
NAMED_UNIT(*)
SI_UNIT($,.STERADIAN.)
SOLID_ANGLE_UNIT()
);
#2863=SHAPE_DEFINITION_REPRESENTATION(#2866,#2871);
#2864=SHAPE_DEFINITION_REPRESENTATION(#2867,#2872);
#2865=SHAPE_DEFINITION_REPRESENTATION(#2868,#2873);
#2866=PRODUCT_DEFINITION_SHAPE('',$,#2875);
#2867=PRODUCT_DEFINITION_SHAPE('',$,#2876);
#2868=PRODUCT_DEFINITION_SHAPE('',$,#2877);
#2869=PRODUCT_DEFINITION_SHAPE($,$,#17);
#2870=PRODUCT_DEFINITION_SHAPE($,$,#18);
#2871=SHAPE_REPRESENTATION('',(#414,#453,#454),#2855);
#2872=SHAPE_REPRESENTATION('',(#415),#2856);
#2873=SHAPE_REPRESENTATION('',(#434),#2857);
#2874=PRODUCT_DEFINITION_CONTEXT('part definition',#2885,'design');
#2875=PRODUCT_DEFINITION('MAT-070','MAT-070',#2878,
#2874);
#2876=PRODUCT_DEFINITION('Hopper','Hopper',#2879,#2874);
#2877=PRODUCT_DEFINITION('Screw Feeder','Screw Feeder',#2880,#2874);
#2878=PRODUCT_DEFINITION_FORMATION('',$,#2887);
#2879=PRODUCT_DEFINITION_FORMATION('',$,#2888);
#2880=PRODUCT_DEFINITION_FORMATION('',$,#2889);
#2881=PRODUCT_RELATED_PRODUCT_CATEGORY('MAT-070',
'MAT-070',(#2887));
#2882=PRODUCT_RELATED_PRODUCT_CATEGORY('Hopper','Hopper',(#2888));
#2883=PRODUCT_RELATED_PRODUCT_CATEGORY('Screw Feeder','Screw Feeder',(#2889));
#2884=APPLICATION_PROTOCOL_DEFINITION('international standard',
'automotive_design',2009,#2885);
#2885=APPLICATION_CONTEXT(
'Core Data for Automotive Mechanical Design Process');
#2886=PRODUCT_CONTEXT('part definition',#2885,'mechanical');
#2887=PRODUCT('MAT-070','MAT-070',$,(#2886));
#2888=PRODUCT('Hopper','Hopper',$,(#2886));
#2889=PRODUCT('Screw Feeder','Screw Feeder',$,(#2886));
#2890=PRESENTATION_STYLE_ASSIGNMENT((#2891));
#2891=SURFACE_STYLE_USAGE(.BOTH.,#2892);
#2892=SURFACE_SIDE_STYLE('',(#2893));
#2893=SURFACE_STYLE_FILL_AREA(#2894);
#2894=FILL_AREA_STYLE('Steel - Satin',(#2895));
#2895=FILL_AREA_STYLE_COLOUR('Steel - Satin',#2896);
#2896=COLOUR_RGB('Steel - Satin',0.627450980392157,0.627450980392157,0.627450980392157);
ENDSEC;
END-ISO-10303-21;
